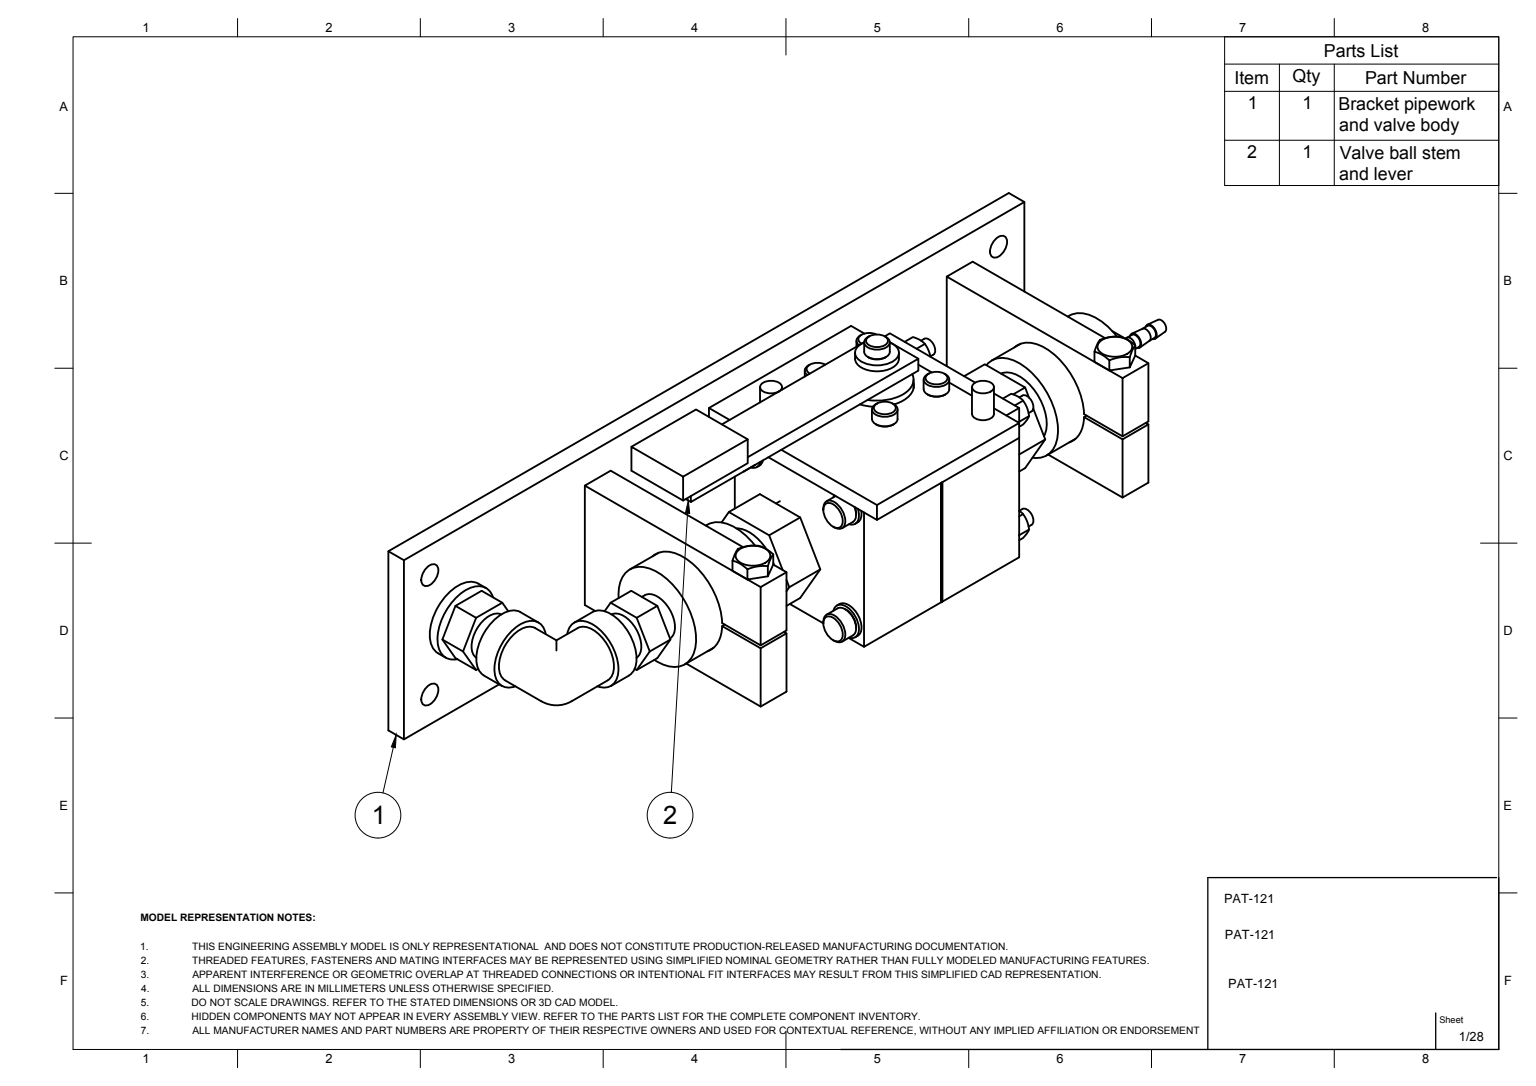
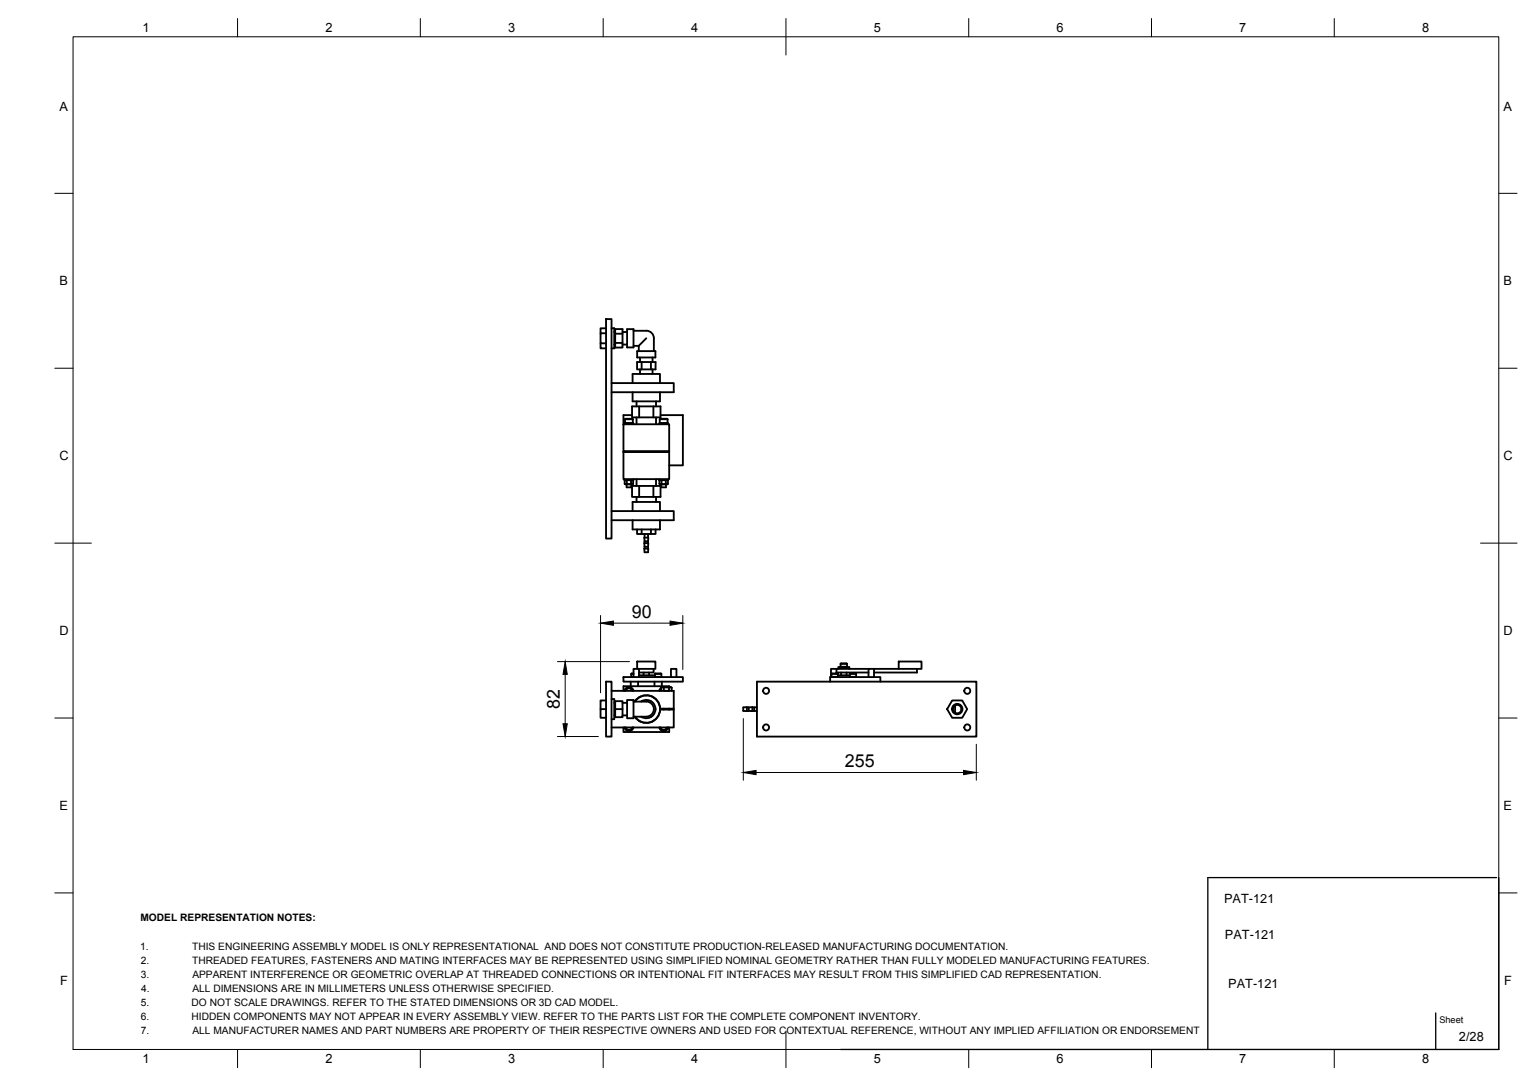
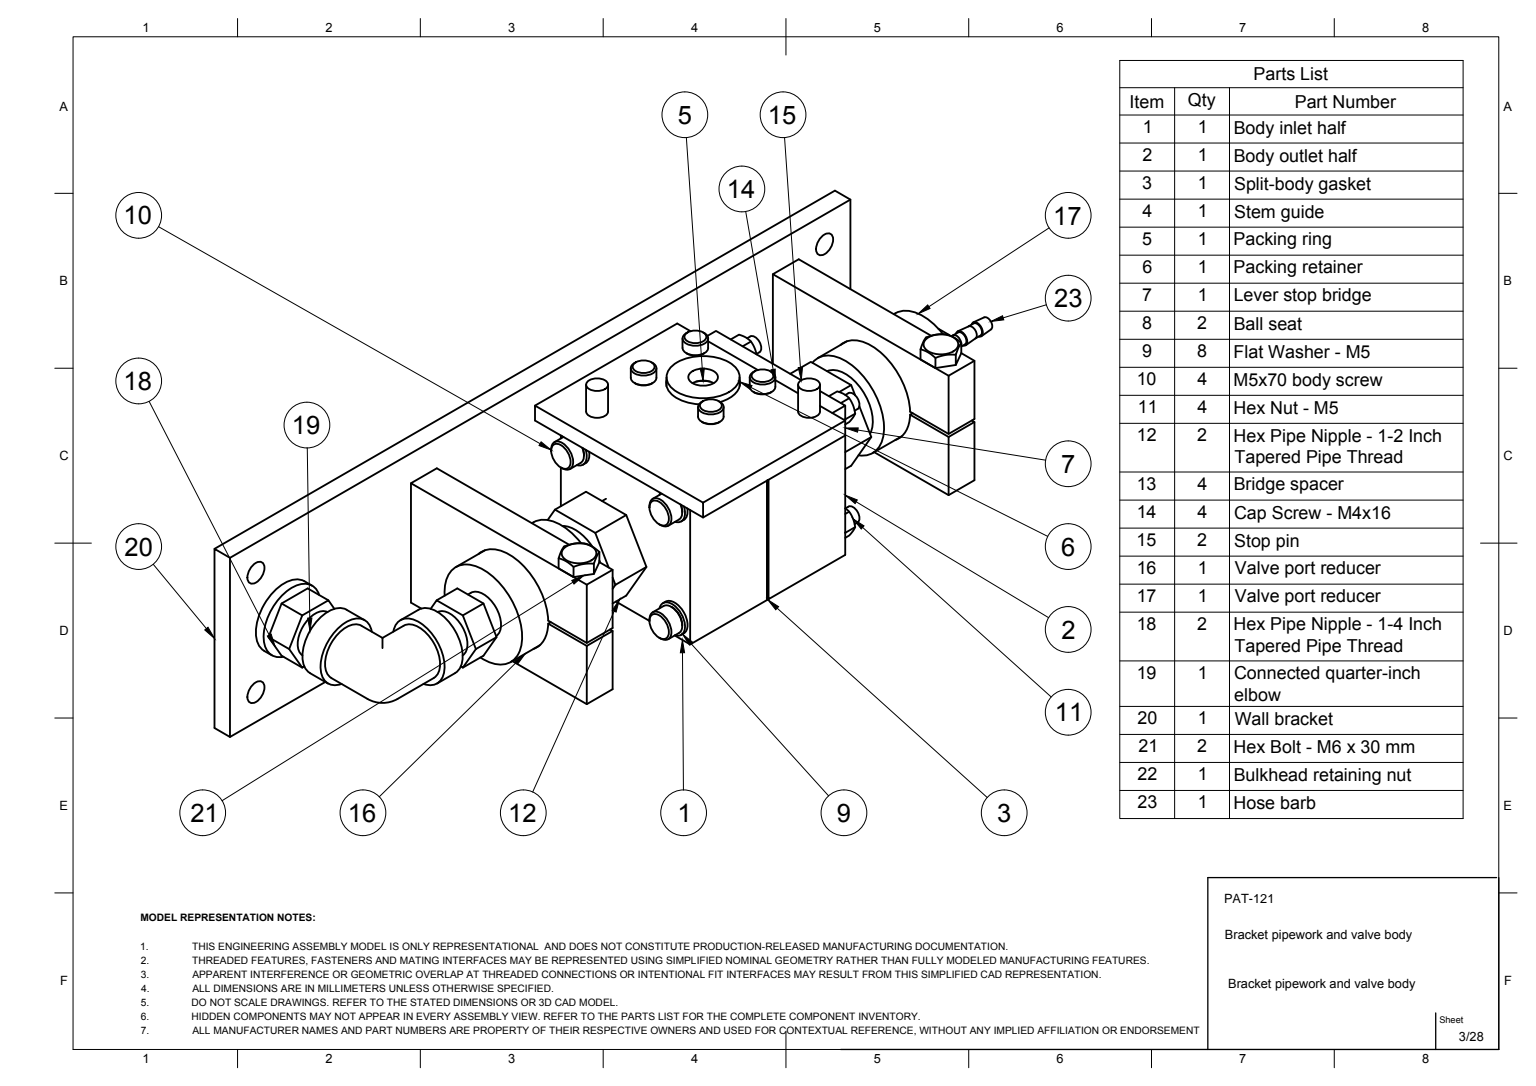
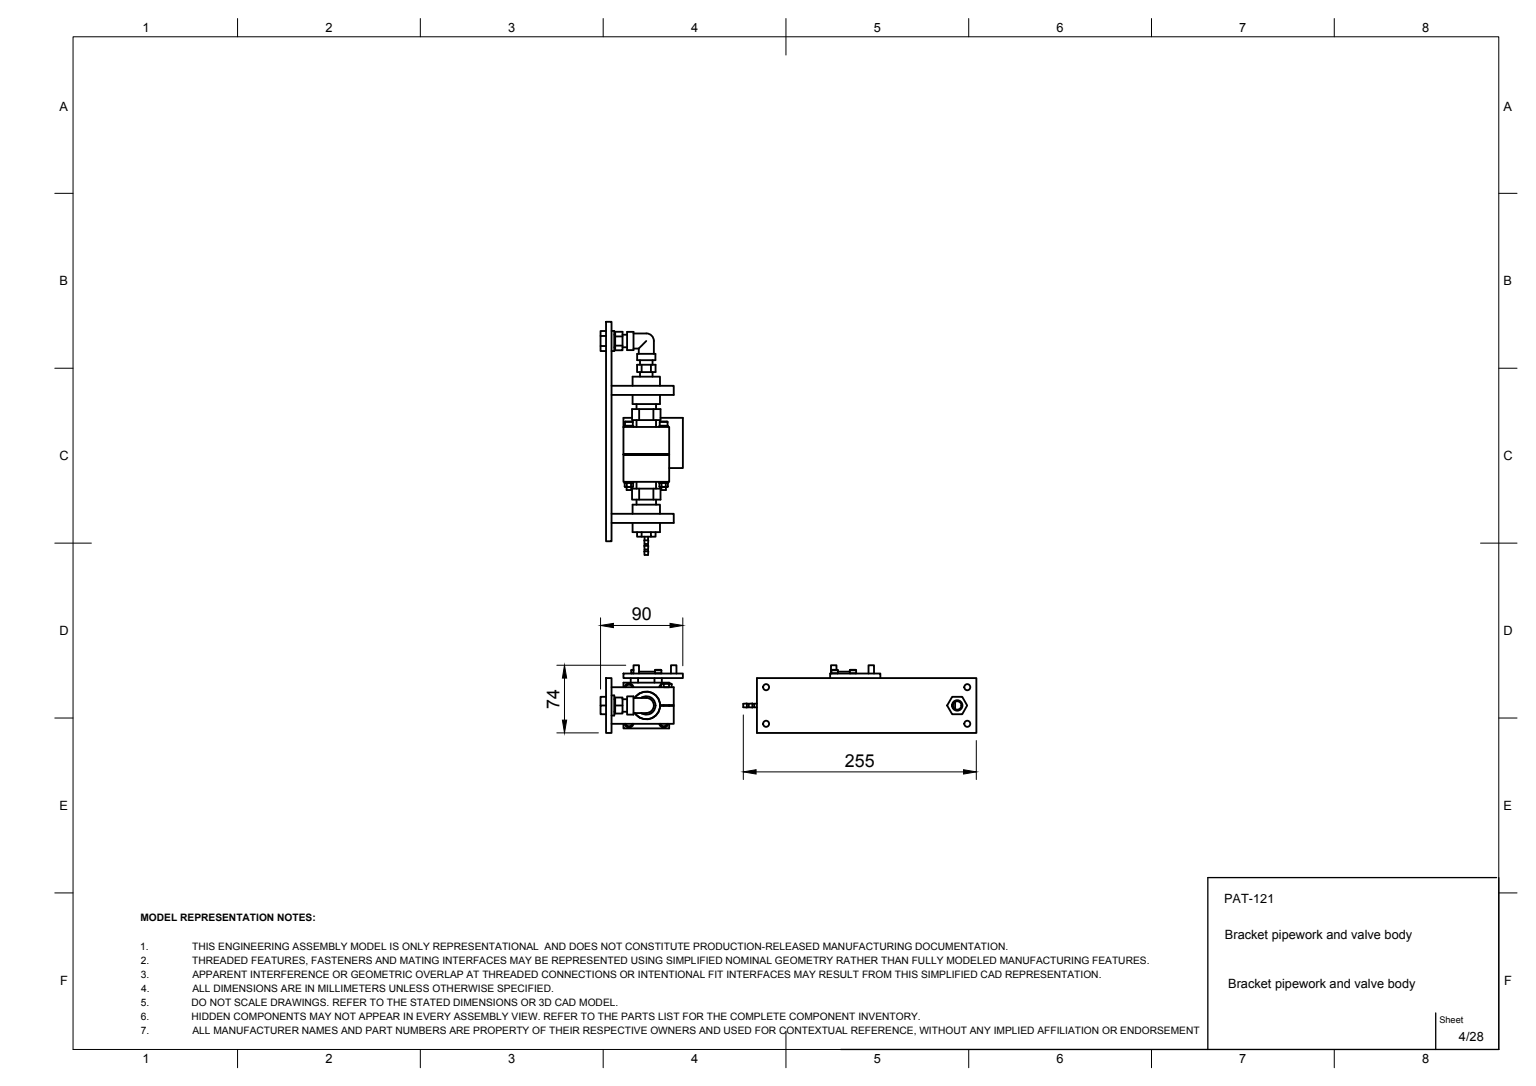
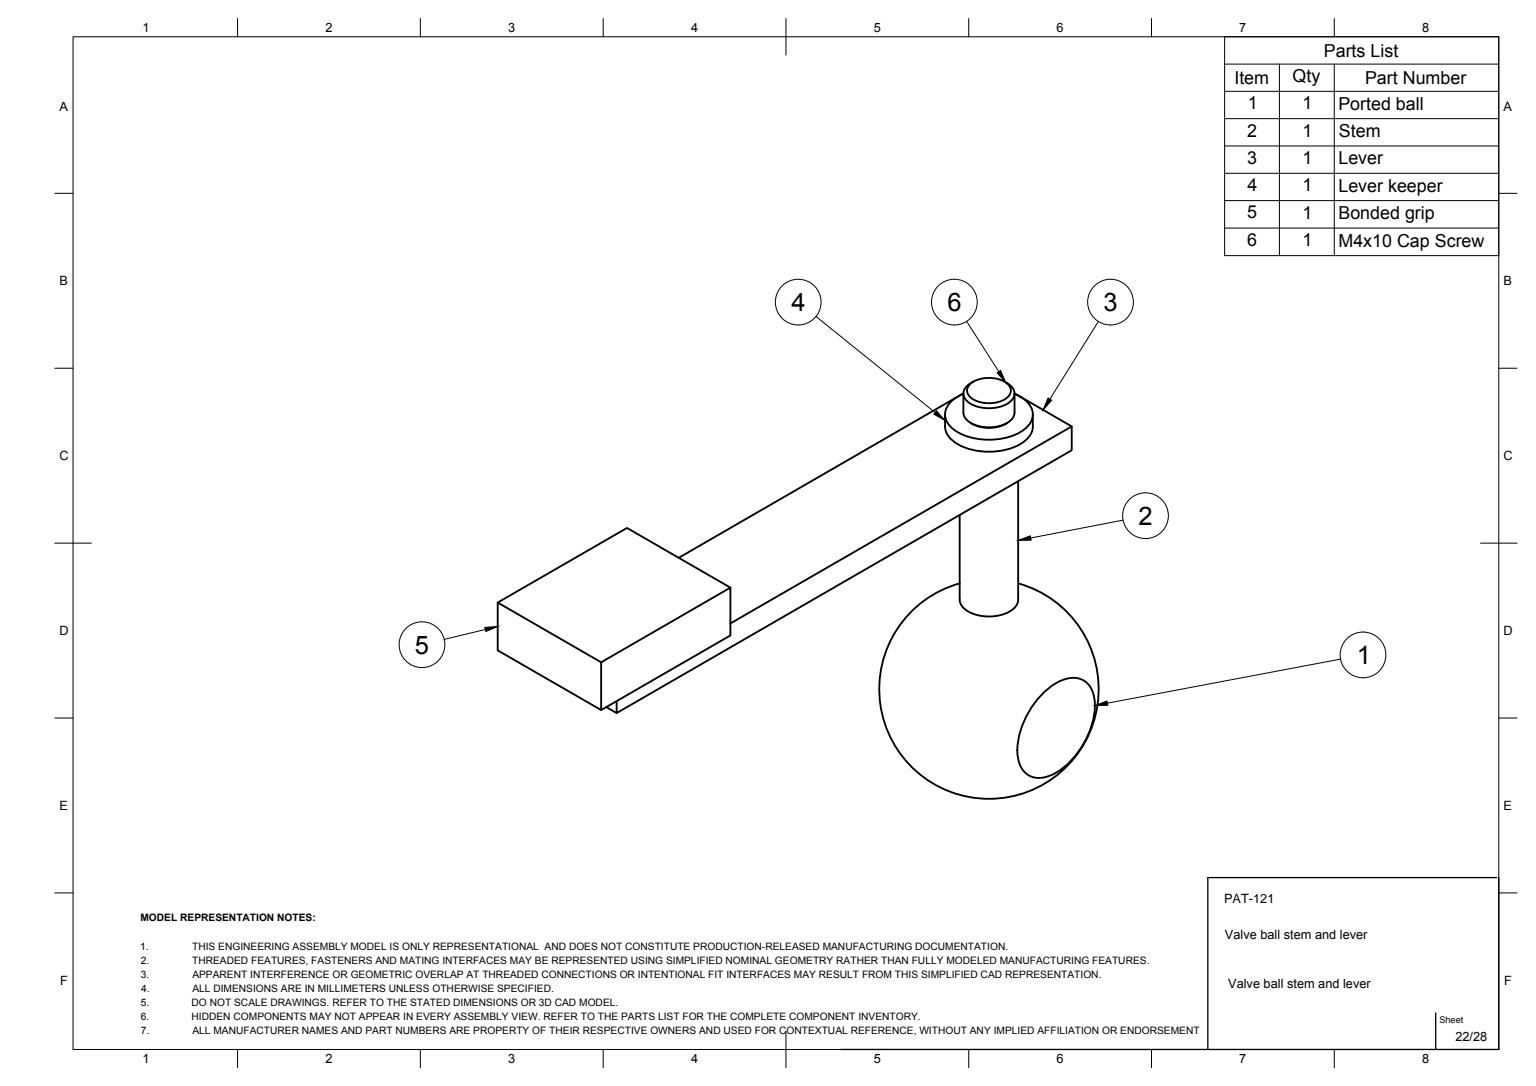
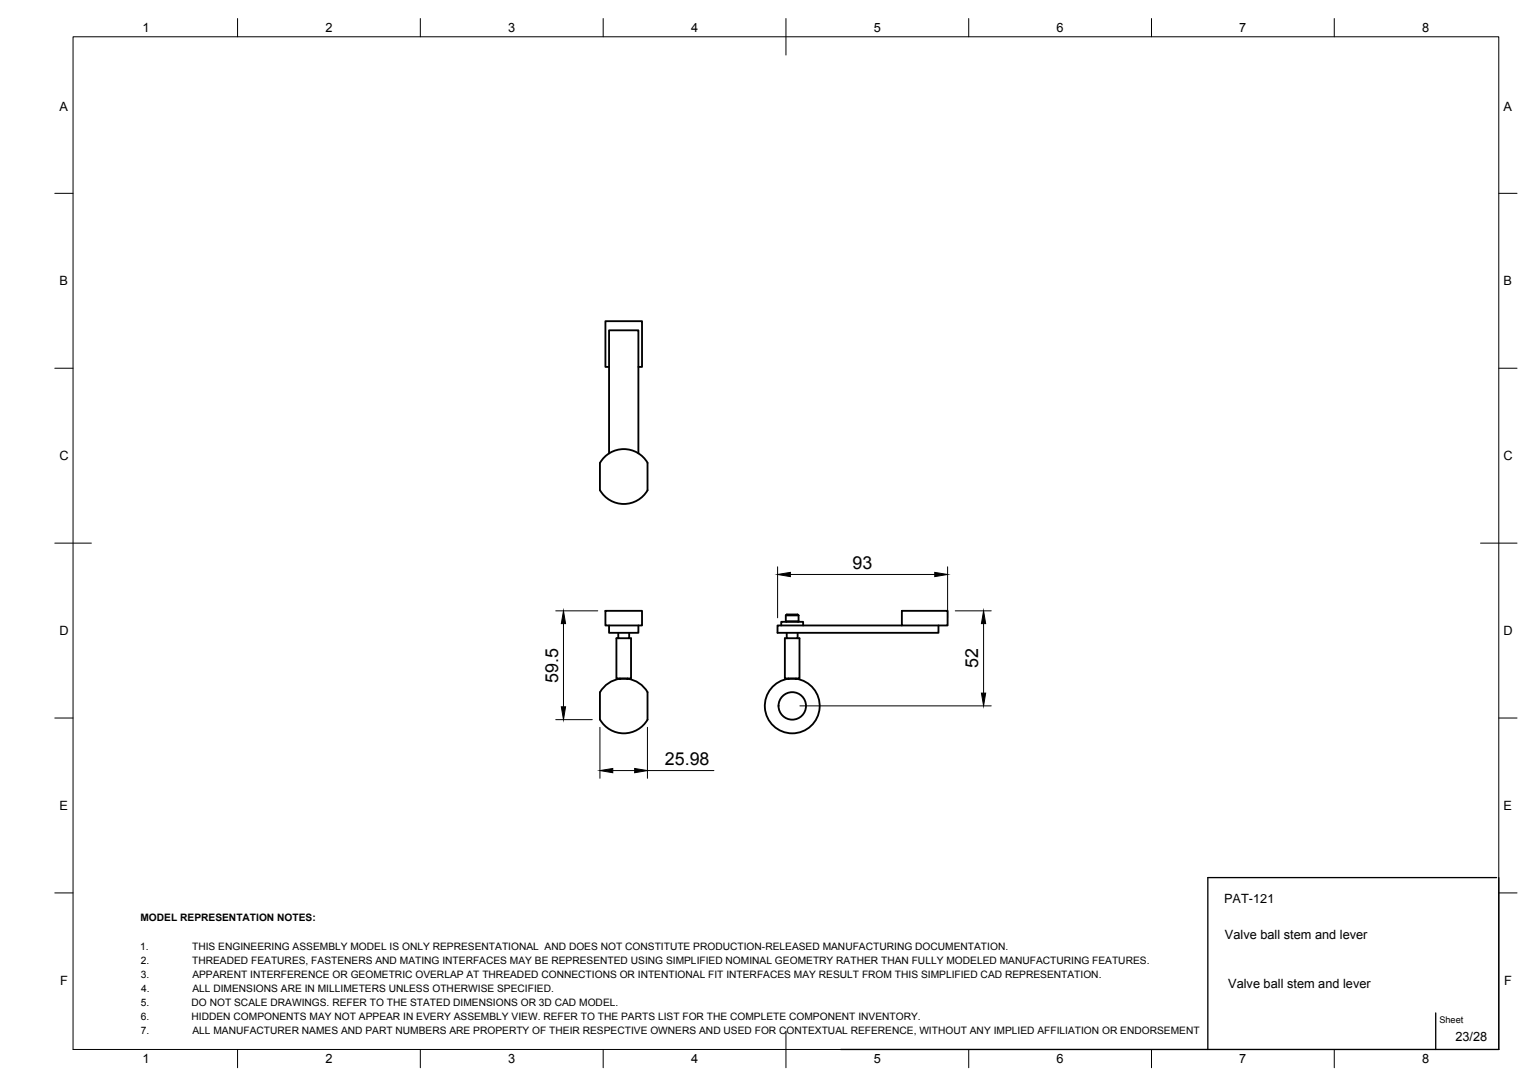
ISO-10303-21;
HEADER;
/* Generated by software containing ST-Developer
 * from STEP Tools, Inc. (www.steptools.com) 
 */

FILE_DESCRIPTION(
/* description */ ('Wall-mounted air drop station'),
/* implementation_level */ '2;1');

FILE_NAME(
/* name */ 'PAT-121',
/* time_stamp */ '2026-10-28T22:16:19-07:00',
/* author */ (''),
/* organization */ (''),
/* preprocessor_version */ 'ST-DEVELOPER v20.2',
/* originating_system */ 'Autodesk Translation Framework v15.17.0.0',
/* authorisation */ '');

FILE_SCHEMA (('AUTOMOTIVE_DESIGN { 1 0 10303 214 3 1 1 }'));
ENDSEC;

DATA;
#10=MECHANICAL_DESIGN_GEOMETRIC_PRESENTATION_REPRESENTATION('',(#344,#345,
#346,#347,#348,#349,#350,#351,#352,#353,#354,#355,#356,#357,#358,#359,#360,
#361,#362,#363,#364,#365,#366,#367,#368,#369,#370,#371,#372),#10517);
#11=ITEM_DEFINED_TRANSFORMATION($,$,#6237,#6766);
#12=ITEM_DEFINED_TRANSFORMATION($,$,#6254,#6767);
#13=ITEM_DEFINED_TRANSFORMATION($,$,#6271,#6768);
#14=ITEM_DEFINED_TRANSFORMATION($,$,#6333,#6769);
#15=ITEM_DEFINED_TRANSFORMATION($,$,#6345,#6770);
#16=ITEM_DEFINED_TRANSFORMATION($,$,#6381,#6771);
#17=ITEM_DEFINED_TRANSFORMATION($,$,#6424,#6772);
#18=ITEM_DEFINED_TRANSFORMATION($,$,#6467,#6773);
#19=ITEM_DEFINED_TRANSFORMATION($,$,#6494,#6774);
#20=ITEM_DEFINED_TRANSFORMATION($,$,#6507,#6775);
#21=ITEM_DEFINED_TRANSFORMATION($,$,#6511,#6776);
#22=ITEM_DEFINED_TRANSFORMATION($,$,#6524,#6777);
#23=ITEM_DEFINED_TRANSFORMATION($,$,#6554,#6778);
#24=ITEM_DEFINED_TRANSFORMATION($,$,#6554,#6779);
#25=ITEM_DEFINED_TRANSFORMATION($,$,#6593,#6780);
#26=ITEM_DEFINED_TRANSFORMATION($,$,#6565,#6781);
#27=ITEM_DEFINED_TRANSFORMATION($,$,#6593,#6782);
#28=ITEM_DEFINED_TRANSFORMATION($,$,#6604,#6783);
#29=ITEM_DEFINED_TRANSFORMATION($,$,#6593,#6784);
#30=ITEM_DEFINED_TRANSFORMATION($,$,#6565,#6785);
#31=ITEM_DEFINED_TRANSFORMATION($,$,#6593,#6786);
#32=ITEM_DEFINED_TRANSFORMATION($,$,#6604,#6787);
#33=ITEM_DEFINED_TRANSFORMATION($,$,#6593,#6788);
#34=ITEM_DEFINED_TRANSFORMATION($,$,#6565,#6789);
#35=ITEM_DEFINED_TRANSFORMATION($,$,#6593,#6790);
#36=ITEM_DEFINED_TRANSFORMATION($,$,#6604,#6791);
#37=ITEM_DEFINED_TRANSFORMATION($,$,#6593,#6792);
#38=ITEM_DEFINED_TRANSFORMATION($,$,#6565,#6793);
#39=ITEM_DEFINED_TRANSFORMATION($,$,#6593,#6794);
#40=ITEM_DEFINED_TRANSFORMATION($,$,#6604,#6795);
#41=ITEM_DEFINED_TRANSFORMATION($,$,#6620,#6796);
#42=ITEM_DEFINED_TRANSFORMATION($,$,#6620,#6797);
#43=ITEM_DEFINED_TRANSFORMATION($,$,#6644,#6798);
#44=ITEM_DEFINED_TRANSFORMATION($,$,#6653,#6799);
#45=ITEM_DEFINED_TRANSFORMATION($,$,#6644,#6800);
#46=ITEM_DEFINED_TRANSFORMATION($,$,#6653,#6801);
#47=ITEM_DEFINED_TRANSFORMATION($,$,#6644,#6802);
#48=ITEM_DEFINED_TRANSFORMATION($,$,#6653,#6803);
#49=ITEM_DEFINED_TRANSFORMATION($,$,#6644,#6804);
#50=ITEM_DEFINED_TRANSFORMATION($,$,#6653,#6805);
#51=ITEM_DEFINED_TRANSFORMATION($,$,#6679,#6806);
#52=ITEM_DEFINED_TRANSFORMATION($,$,#6679,#6807);
#53=ITEM_DEFINED_TRANSFORMATION($,$,#6725,#6808);
#54=ITEM_DEFINED_TRANSFORMATION($,$,#6685,#6809);
#55=ITEM_DEFINED_TRANSFORMATION($,$,#6725,#6810);
#56=ITEM_DEFINED_TRANSFORMATION($,$,#6749,#6811);
#57=ITEM_DEFINED_TRANSFORMATION($,$,#6749,#6812);
#58=ITEM_DEFINED_TRANSFORMATION($,$,#6814,#6916);
#59=ITEM_DEFINED_TRANSFORMATION($,$,#6830,#6917);
#60=ITEM_DEFINED_TRANSFORMATION($,$,#6865,#6918);
#61=ITEM_DEFINED_TRANSFORMATION($,$,#6876,#6919);
#62=ITEM_DEFINED_TRANSFORMATION($,$,#6885,#6920);
#63=ITEM_DEFINED_TRANSFORMATION($,$,#6892,#6921);
#64=ITEM_DEFINED_TRANSFORMATION($,$,#6236,#6922);
#65=ITEM_DEFINED_TRANSFORMATION($,$,#6813,#6923);
#66=(
REPRESENTATION_RELATIONSHIP($,$,#10643,#10642)
REPRESENTATION_RELATIONSHIP_WITH_TRANSFORMATION(#11)
SHAPE_REPRESENTATION_RELATIONSHIP()
);
#67=(
REPRESENTATION_RELATIONSHIP($,$,#10644,#10642)
REPRESENTATION_RELATIONSHIP_WITH_TRANSFORMATION(#12)
SHAPE_REPRESENTATION_RELATIONSHIP()
);
#68=(
REPRESENTATION_RELATIONSHIP($,$,#10645,#10642)
REPRESENTATION_RELATIONSHIP_WITH_TRANSFORMATION(#13)
SHAPE_REPRESENTATION_RELATIONSHIP()
);
#69=(
REPRESENTATION_RELATIONSHIP($,$,#10646,#10642)
REPRESENTATION_RELATIONSHIP_WITH_TRANSFORMATION(#14)
SHAPE_REPRESENTATION_RELATIONSHIP()
);
#70=(
REPRESENTATION_RELATIONSHIP($,$,#10647,#10642)
REPRESENTATION_RELATIONSHIP_WITH_TRANSFORMATION(#15)
SHAPE_REPRESENTATION_RELATIONSHIP()
);
#71=(
REPRESENTATION_RELATIONSHIP($,$,#10648,#10642)
REPRESENTATION_RELATIONSHIP_WITH_TRANSFORMATION(#16)
SHAPE_REPRESENTATION_RELATIONSHIP()
);
#72=(
REPRESENTATION_RELATIONSHIP($,$,#10649,#10642)
REPRESENTATION_RELATIONSHIP_WITH_TRANSFORMATION(#17)
SHAPE_REPRESENTATION_RELATIONSHIP()
);
#73=(
REPRESENTATION_RELATIONSHIP($,$,#10650,#10642)
REPRESENTATION_RELATIONSHIP_WITH_TRANSFORMATION(#18)
SHAPE_REPRESENTATION_RELATIONSHIP()
);
#74=(
REPRESENTATION_RELATIONSHIP($,$,#10651,#10642)
REPRESENTATION_RELATIONSHIP_WITH_TRANSFORMATION(#19)
SHAPE_REPRESENTATION_RELATIONSHIP()
);
#75=(
REPRESENTATION_RELATIONSHIP($,$,#10652,#10642)
REPRESENTATION_RELATIONSHIP_WITH_TRANSFORMATION(#20)
SHAPE_REPRESENTATION_RELATIONSHIP()
);
#76=(
REPRESENTATION_RELATIONSHIP($,$,#10653,#10642)
REPRESENTATION_RELATIONSHIP_WITH_TRANSFORMATION(#21)
SHAPE_REPRESENTATION_RELATIONSHIP()
);
#77=(
REPRESENTATION_RELATIONSHIP($,$,#10654,#10642)
REPRESENTATION_RELATIONSHIP_WITH_TRANSFORMATION(#22)
SHAPE_REPRESENTATION_RELATIONSHIP()
);
#78=(
REPRESENTATION_RELATIONSHIP($,$,#10655,#10642)
REPRESENTATION_RELATIONSHIP_WITH_TRANSFORMATION(#23)
SHAPE_REPRESENTATION_RELATIONSHIP()
);
#79=(
REPRESENTATION_RELATIONSHIP($,$,#10655,#10642)
REPRESENTATION_RELATIONSHIP_WITH_TRANSFORMATION(#24)
SHAPE_REPRESENTATION_RELATIONSHIP()
);
#80=(
REPRESENTATION_RELATIONSHIP($,$,#10657,#10642)
REPRESENTATION_RELATIONSHIP_WITH_TRANSFORMATION(#25)
SHAPE_REPRESENTATION_RELATIONSHIP()
);
#81=(
REPRESENTATION_RELATIONSHIP($,$,#10656,#10642)
REPRESENTATION_RELATIONSHIP_WITH_TRANSFORMATION(#26)
SHAPE_REPRESENTATION_RELATIONSHIP()
);
#82=(
REPRESENTATION_RELATIONSHIP($,$,#10657,#10642)
REPRESENTATION_RELATIONSHIP_WITH_TRANSFORMATION(#27)
SHAPE_REPRESENTATION_RELATIONSHIP()
);
#83=(
REPRESENTATION_RELATIONSHIP($,$,#10658,#10642)
REPRESENTATION_RELATIONSHIP_WITH_TRANSFORMATION(#28)
SHAPE_REPRESENTATION_RELATIONSHIP()
);
#84=(
REPRESENTATION_RELATIONSHIP($,$,#10657,#10642)
REPRESENTATION_RELATIONSHIP_WITH_TRANSFORMATION(#29)
SHAPE_REPRESENTATION_RELATIONSHIP()
);
#85=(
REPRESENTATION_RELATIONSHIP($,$,#10656,#10642)
REPRESENTATION_RELATIONSHIP_WITH_TRANSFORMATION(#30)
SHAPE_REPRESENTATION_RELATIONSHIP()
);
#86=(
REPRESENTATION_RELATIONSHIP($,$,#10657,#10642)
REPRESENTATION_RELATIONSHIP_WITH_TRANSFORMATION(#31)
SHAPE_REPRESENTATION_RELATIONSHIP()
);
#87=(
REPRESENTATION_RELATIONSHIP($,$,#10658,#10642)
REPRESENTATION_RELATIONSHIP_WITH_TRANSFORMATION(#32)
SHAPE_REPRESENTATION_RELATIONSHIP()
);
#88=(
REPRESENTATION_RELATIONSHIP($,$,#10657,#10642)
REPRESENTATION_RELATIONSHIP_WITH_TRANSFORMATION(#33)
SHAPE_REPRESENTATION_RELATIONSHIP()
);
#89=(
REPRESENTATION_RELATIONSHIP($,$,#10656,#10642)
REPRESENTATION_RELATIONSHIP_WITH_TRANSFORMATION(#34)
SHAPE_REPRESENTATION_RELATIONSHIP()
);
#90=(
REPRESENTATION_RELATIONSHIP($,$,#10657,#10642)
REPRESENTATION_RELATIONSHIP_WITH_TRANSFORMATION(#35)
SHAPE_REPRESENTATION_RELATIONSHIP()
);
#91=(
REPRESENTATION_RELATIONSHIP($,$,#10658,#10642)
REPRESENTATION_RELATIONSHIP_WITH_TRANSFORMATION(#36)
SHAPE_REPRESENTATION_RELATIONSHIP()
);
#92=(
REPRESENTATION_RELATIONSHIP($,$,#10657,#10642)
REPRESENTATION_RELATIONSHIP_WITH_TRANSFORMATION(#37)
SHAPE_REPRESENTATION_RELATIONSHIP()
);
#93=(
REPRESENTATION_RELATIONSHIP($,$,#10656,#10642)
REPRESENTATION_RELATIONSHIP_WITH_TRANSFORMATION(#38)
SHAPE_REPRESENTATION_RELATIONSHIP()
);
#94=(
REPRESENTATION_RELATIONSHIP($,$,#10657,#10642)
REPRESENTATION_RELATIONSHIP_WITH_TRANSFORMATION(#39)
SHAPE_REPRESENTATION_RELATIONSHIP()
);
#95=(
REPRESENTATION_RELATIONSHIP($,$,#10658,#10642)
REPRESENTATION_RELATIONSHIP_WITH_TRANSFORMATION(#40)
SHAPE_REPRESENTATION_RELATIONSHIP()
);
#96=(
REPRESENTATION_RELATIONSHIP($,$,#10659,#10642)
REPRESENTATION_RELATIONSHIP_WITH_TRANSFORMATION(#41)
SHAPE_REPRESENTATION_RELATIONSHIP()
);
#97=(
REPRESENTATION_RELATIONSHIP($,$,#10659,#10642)
REPRESENTATION_RELATIONSHIP_WITH_TRANSFORMATION(#42)
SHAPE_REPRESENTATION_RELATIONSHIP()
);
#98=(
REPRESENTATION_RELATIONSHIP($,$,#10660,#10642)
REPRESENTATION_RELATIONSHIP_WITH_TRANSFORMATION(#43)
SHAPE_REPRESENTATION_RELATIONSHIP()
);
#99=(
REPRESENTATION_RELATIONSHIP($,$,#10661,#10642)
REPRESENTATION_RELATIONSHIP_WITH_TRANSFORMATION(#44)
SHAPE_REPRESENTATION_RELATIONSHIP()
);
#100=(
REPRESENTATION_RELATIONSHIP($,$,#10660,#10642)
REPRESENTATION_RELATIONSHIP_WITH_TRANSFORMATION(#45)
SHAPE_REPRESENTATION_RELATIONSHIP()
);
#101=(
REPRESENTATION_RELATIONSHIP($,$,#10661,#10642)
REPRESENTATION_RELATIONSHIP_WITH_TRANSFORMATION(#46)
SHAPE_REPRESENTATION_RELATIONSHIP()
);
#102=(
REPRESENTATION_RELATIONSHIP($,$,#10660,#10642)
REPRESENTATION_RELATIONSHIP_WITH_TRANSFORMATION(#47)
SHAPE_REPRESENTATION_RELATIONSHIP()
);
#103=(
REPRESENTATION_RELATIONSHIP($,$,#10661,#10642)
REPRESENTATION_RELATIONSHIP_WITH_TRANSFORMATION(#48)
SHAPE_REPRESENTATION_RELATIONSHIP()
);
#104=(
REPRESENTATION_RELATIONSHIP($,$,#10660,#10642)
REPRESENTATION_RELATIONSHIP_WITH_TRANSFORMATION(#49)
SHAPE_REPRESENTATION_RELATIONSHIP()
);
#105=(
REPRESENTATION_RELATIONSHIP($,$,#10661,#10642)
REPRESENTATION_RELATIONSHIP_WITH_TRANSFORMATION(#50)
SHAPE_REPRESENTATION_RELATIONSHIP()
);
#106=(
REPRESENTATION_RELATIONSHIP($,$,#10662,#10642)
REPRESENTATION_RELATIONSHIP_WITH_TRANSFORMATION(#51)
SHAPE_REPRESENTATION_RELATIONSHIP()
);
#107=(
REPRESENTATION_RELATIONSHIP($,$,#10662,#10642)
REPRESENTATION_RELATIONSHIP_WITH_TRANSFORMATION(#52)
SHAPE_REPRESENTATION_RELATIONSHIP()
);
#108=(
REPRESENTATION_RELATIONSHIP($,$,#10664,#10642)
REPRESENTATION_RELATIONSHIP_WITH_TRANSFORMATION(#53)
SHAPE_REPRESENTATION_RELATIONSHIP()
);
#109=(
REPRESENTATION_RELATIONSHIP($,$,#10663,#10642)
REPRESENTATION_RELATIONSHIP_WITH_TRANSFORMATION(#54)
SHAPE_REPRESENTATION_RELATIONSHIP()
);
#110=(
REPRESENTATION_RELATIONSHIP($,$,#10664,#10642)
REPRESENTATION_RELATIONSHIP_WITH_TRANSFORMATION(#55)
SHAPE_REPRESENTATION_RELATIONSHIP()
);
#111=(
REPRESENTATION_RELATIONSHIP($,$,#10665,#10642)
REPRESENTATION_RELATIONSHIP_WITH_TRANSFORMATION(#56)
SHAPE_REPRESENTATION_RELATIONSHIP()
);
#112=(
REPRESENTATION_RELATIONSHIP($,$,#10665,#10642)
REPRESENTATION_RELATIONSHIP_WITH_TRANSFORMATION(#57)
SHAPE_REPRESENTATION_RELATIONSHIP()
);
#113=(
REPRESENTATION_RELATIONSHIP($,$,#10667,#10666)
REPRESENTATION_RELATIONSHIP_WITH_TRANSFORMATION(#58)
SHAPE_REPRESENTATION_RELATIONSHIP()
);
#114=(
REPRESENTATION_RELATIONSHIP($,$,#10668,#10666)
REPRESENTATION_RELATIONSHIP_WITH_TRANSFORMATION(#59)
SHAPE_REPRESENTATION_RELATIONSHIP()
);
#115=(
REPRESENTATION_RELATIONSHIP($,$,#10669,#10666)
REPRESENTATION_RELATIONSHIP_WITH_TRANSFORMATION(#60)
SHAPE_REPRESENTATION_RELATIONSHIP()
);
#116=(
REPRESENTATION_RELATIONSHIP($,$,#10670,#10666)
REPRESENTATION_RELATIONSHIP_WITH_TRANSFORMATION(#61)
SHAPE_REPRESENTATION_RELATIONSHIP()
);
#117=(
REPRESENTATION_RELATIONSHIP($,$,#10671,#10666)
REPRESENTATION_RELATIONSHIP_WITH_TRANSFORMATION(#62)
SHAPE_REPRESENTATION_RELATIONSHIP()
);
#118=(
REPRESENTATION_RELATIONSHIP($,$,#10672,#10666)
REPRESENTATION_RELATIONSHIP_WITH_TRANSFORMATION(#63)
SHAPE_REPRESENTATION_RELATIONSHIP()
);
#119=(
REPRESENTATION_RELATIONSHIP($,$,#10642,#10641)
REPRESENTATION_RELATIONSHIP_WITH_TRANSFORMATION(#64)
SHAPE_REPRESENTATION_RELATIONSHIP()
);
#120=(
REPRESENTATION_RELATIONSHIP($,$,#10666,#10641)
REPRESENTATION_RELATIONSHIP_WITH_TRANSFORMATION(#65)
SHAPE_REPRESENTATION_RELATIONSHIP()
);
#121=CONTEXT_DEPENDENT_SHAPE_REPRESENTATION(#66,#10579);
#122=CONTEXT_DEPENDENT_SHAPE_REPRESENTATION(#67,#10580);
#123=CONTEXT_DEPENDENT_SHAPE_REPRESENTATION(#68,#10581);
#124=CONTEXT_DEPENDENT_SHAPE_REPRESENTATION(#69,#10582);
#125=CONTEXT_DEPENDENT_SHAPE_REPRESENTATION(#70,#10583);
#126=CONTEXT_DEPENDENT_SHAPE_REPRESENTATION(#71,#10584);
#127=CONTEXT_DEPENDENT_SHAPE_REPRESENTATION(#72,#10585);
#128=CONTEXT_DEPENDENT_SHAPE_REPRESENTATION(#73,#10586);
#129=CONTEXT_DEPENDENT_SHAPE_REPRESENTATION(#74,#10587);
#130=CONTEXT_DEPENDENT_SHAPE_REPRESENTATION(#75,#10588);
#131=CONTEXT_DEPENDENT_SHAPE_REPRESENTATION(#76,#10589);
#132=CONTEXT_DEPENDENT_SHAPE_REPRESENTATION(#77,#10590);
#133=CONTEXT_DEPENDENT_SHAPE_REPRESENTATION(#78,#10591);
#134=CONTEXT_DEPENDENT_SHAPE_REPRESENTATION(#79,#10592);
#135=CONTEXT_DEPENDENT_SHAPE_REPRESENTATION(#80,#10593);
#136=CONTEXT_DEPENDENT_SHAPE_REPRESENTATION(#81,#10594);
#137=CONTEXT_DEPENDENT_SHAPE_REPRESENTATION(#82,#10595);
#138=CONTEXT_DEPENDENT_SHAPE_REPRESENTATION(#83,#10596);
#139=CONTEXT_DEPENDENT_SHAPE_REPRESENTATION(#84,#10597);
#140=CONTEXT_DEPENDENT_SHAPE_REPRESENTATION(#85,#10598);
#141=CONTEXT_DEPENDENT_SHAPE_REPRESENTATION(#86,#10599);
#142=CONTEXT_DEPENDENT_SHAPE_REPRESENTATION(#87,#10600);
#143=CONTEXT_DEPENDENT_SHAPE_REPRESENTATION(#88,#10601);
#144=CONTEXT_DEPENDENT_SHAPE_REPRESENTATION(#89,#10602);
#145=CONTEXT_DEPENDENT_SHAPE_REPRESENTATION(#90,#10603);
#146=CONTEXT_DEPENDENT_SHAPE_REPRESENTATION(#91,#10604);
#147=CONTEXT_DEPENDENT_SHAPE_REPRESENTATION(#92,#10605);
#148=CONTEXT_DEPENDENT_SHAPE_REPRESENTATION(#93,#10606);
#149=CONTEXT_DEPENDENT_SHAPE_REPRESENTATION(#94,#10607);
#150=CONTEXT_DEPENDENT_SHAPE_REPRESENTATION(#95,#10608);
#151=CONTEXT_DEPENDENT_SHAPE_REPRESENTATION(#96,#10609);
#152=CONTEXT_DEPENDENT_SHAPE_REPRESENTATION(#97,#10610);
#153=CONTEXT_DEPENDENT_SHAPE_REPRESENTATION(#98,#10611);
#154=CONTEXT_DEPENDENT_SHAPE_REPRESENTATION(#99,#10612);
#155=CONTEXT_DEPENDENT_SHAPE_REPRESENTATION(#100,#10613);
#156=CONTEXT_DEPENDENT_SHAPE_REPRESENTATION(#101,#10614);
#157=CONTEXT_DEPENDENT_SHAPE_REPRESENTATION(#102,#10615);
#158=CONTEXT_DEPENDENT_SHAPE_REPRESENTATION(#103,#10616);
#159=CONTEXT_DEPENDENT_SHAPE_REPRESENTATION(#104,#10617);
#160=CONTEXT_DEPENDENT_SHAPE_REPRESENTATION(#105,#10618);
#161=CONTEXT_DEPENDENT_SHAPE_REPRESENTATION(#106,#10619);
#162=CONTEXT_DEPENDENT_SHAPE_REPRESENTATION(#107,#10620);
#163=CONTEXT_DEPENDENT_SHAPE_REPRESENTATION(#108,#10621);
#164=CONTEXT_DEPENDENT_SHAPE_REPRESENTATION(#109,#10622);
#165=CONTEXT_DEPENDENT_SHAPE_REPRESENTATION(#110,#10623);
#166=CONTEXT_DEPENDENT_SHAPE_REPRESENTATION(#111,#10624);
#167=CONTEXT_DEPENDENT_SHAPE_REPRESENTATION(#112,#10625);
#168=CONTEXT_DEPENDENT_SHAPE_REPRESENTATION(#113,#10633);
#169=CONTEXT_DEPENDENT_SHAPE_REPRESENTATION(#114,#10634);
#170=CONTEXT_DEPENDENT_SHAPE_REPRESENTATION(#115,#10635);
#171=CONTEXT_DEPENDENT_SHAPE_REPRESENTATION(#116,#10636);
#172=CONTEXT_DEPENDENT_SHAPE_REPRESENTATION(#117,#10637);
#173=CONTEXT_DEPENDENT_SHAPE_REPRESENTATION(#118,#10638);
#174=CONTEXT_DEPENDENT_SHAPE_REPRESENTATION(#119,#10639);
#175=CONTEXT_DEPENDENT_SHAPE_REPRESENTATION(#120,#10640);
#176=NEXT_ASSEMBLY_USAGE_OCCURRENCE('Valve port reducer:1',
'Valve port reducer:1','Valve port reducer:1',#10675,#10676,
'Valve port reducer:1');
#177=NEXT_ASSEMBLY_USAGE_OCCURRENCE('Valve port reducer (1):1',
'Valve port reducer (1):1','Valve port reducer (1):1',#10675,#10677,
'Valve port reducer (1):1');
#178=NEXT_ASSEMBLY_USAGE_OCCURRENCE('Wall bracket:1','Wall bracket:1',
'Wall bracket:1',#10675,#10678,'Wall bracket:1');
#179=NEXT_ASSEMBLY_USAGE_OCCURRENCE('Bulkhead retaining nut:1',
'Bulkhead retaining nut:1','Bulkhead retaining nut:1',#10675,#10679,
'Bulkhead retaining nut:1');
#180=NEXT_ASSEMBLY_USAGE_OCCURRENCE('Hose barb:1','Hose barb:1',
'Hose barb:1',#10675,#10680,'Hose barb:1');
#181=NEXT_ASSEMBLY_USAGE_OCCURRENCE('Body inlet half:2',
'Body inlet half:2','Body inlet half:2',#10675,#10681,
'Body inlet half:2');
#182=NEXT_ASSEMBLY_USAGE_OCCURRENCE('Body outlet half:2',
'Body outlet half:2','Body outlet half:2',#10675,#10682,
'Body outlet half:2');
#183=NEXT_ASSEMBLY_USAGE_OCCURRENCE('Split-body gasket:2',
'Split-body gasket:2','Split-body gasket:2',#10675,#10683,
'Split-body gasket:2');
#184=NEXT_ASSEMBLY_USAGE_OCCURRENCE('Stem guide:2','Stem guide:2',
'Stem guide:2',#10675,#10684,'Stem guide:2');
#185=NEXT_ASSEMBLY_USAGE_OCCURRENCE('Packing ring:2','Packing ring:2',
'Packing ring:2',#10675,#10685,'Packing ring:2');
#186=NEXT_ASSEMBLY_USAGE_OCCURRENCE('Packing retainer:2',
'Packing retainer:2','Packing retainer:2',#10675,#10686,
'Packing retainer:2');
#187=NEXT_ASSEMBLY_USAGE_OCCURRENCE('Lever stop bridge:2',
'Lever stop bridge:2','Lever stop bridge:2',#10675,#10687,
'Lever stop bridge:2');
#188=NEXT_ASSEMBLY_USAGE_OCCURRENCE('Ball seat:2','Ball seat:2',
'Ball seat:2',#10675,#10688,'Ball seat:2');
#189=NEXT_ASSEMBLY_USAGE_OCCURRENCE('Ball seat:3','Ball seat:3',
'Ball seat:3',#10675,#10688,'Ball seat:3');
#190=NEXT_ASSEMBLY_USAGE_OCCURRENCE('Flat Washer - M5:2',
'Flat Washer - M5:2','Flat Washer - M5:2',#10675,#10690,
'Flat Washer - M5:2');
#191=NEXT_ASSEMBLY_USAGE_OCCURRENCE('M5x70 body screw:2',
'M5x70 body screw:2','M5x70 body screw:2',#10675,#10689,
'M5x70 body screw:2');
#192=NEXT_ASSEMBLY_USAGE_OCCURRENCE('Flat Washer - M5:3',
'Flat Washer - M5:3','Flat Washer - M5:3',#10675,#10690,
'Flat Washer - M5:3');
#193=NEXT_ASSEMBLY_USAGE_OCCURRENCE('Hex Nut - M5:2','Hex Nut - M5:2',
'Hex Nut - M5:2',#10675,#10691,'Hex Nut - M5:2');
#194=NEXT_ASSEMBLY_USAGE_OCCURRENCE('Flat Washer - M5:4',
'Flat Washer - M5:4','Flat Washer - M5:4',#10675,#10690,
'Flat Washer - M5:4');
#195=NEXT_ASSEMBLY_USAGE_OCCURRENCE('M5x70 body screw:3',
'M5x70 body screw:3','M5x70 body screw:3',#10675,#10689,
'M5x70 body screw:3');
#196=NEXT_ASSEMBLY_USAGE_OCCURRENCE('Flat Washer - M5:5',
'Flat Washer - M5:5','Flat Washer - M5:5',#10675,#10690,
'Flat Washer - M5:5');
#197=NEXT_ASSEMBLY_USAGE_OCCURRENCE('Hex Nut - M5:3','Hex Nut - M5:3',
'Hex Nut - M5:3',#10675,#10691,'Hex Nut - M5:3');
#198=NEXT_ASSEMBLY_USAGE_OCCURRENCE('Flat Washer - M5:6',
'Flat Washer - M5:6','Flat Washer - M5:6',#10675,#10690,
'Flat Washer - M5:6');
#199=NEXT_ASSEMBLY_USAGE_OCCURRENCE('M5x70 body screw:4',
'M5x70 body screw:4','M5x70 body screw:4',#10675,#10689,
'M5x70 body screw:4');
#200=NEXT_ASSEMBLY_USAGE_OCCURRENCE('Flat Washer - M5:7',
'Flat Washer - M5:7','Flat Washer - M5:7',#10675,#10690,
'Flat Washer - M5:7');
#201=NEXT_ASSEMBLY_USAGE_OCCURRENCE('Hex Nut - M5:4','Hex Nut - M5:4',
'Hex Nut - M5:4',#10675,#10691,'Hex Nut - M5:4');
#202=NEXT_ASSEMBLY_USAGE_OCCURRENCE('Flat Washer - M5:8',
'Flat Washer - M5:8','Flat Washer - M5:8',#10675,#10690,
'Flat Washer - M5:8');
#203=NEXT_ASSEMBLY_USAGE_OCCURRENCE('M5x70 body screw:5',
'M5x70 body screw:5','M5x70 body screw:5',#10675,#10689,
'M5x70 body screw:5');
#204=NEXT_ASSEMBLY_USAGE_OCCURRENCE('Flat Washer - M5:9',
'Flat Washer - M5:9','Flat Washer - M5:9',#10675,#10690,
'Flat Washer - M5:9');
#205=NEXT_ASSEMBLY_USAGE_OCCURRENCE('Hex Nut - M5:5','Hex Nut - M5:5',
'Hex Nut - M5:5',#10675,#10691,'Hex Nut - M5:5');
#206=NEXT_ASSEMBLY_USAGE_OCCURRENCE(
'Hex Pipe Nipple - 1-2 Inch Tapered Pipe Thread:2',
'Hex Pipe Nipple - 1-2 Inch Tapered Pipe Thread:2',
'Hex Pipe Nipple - 1-2 Inch Tapered Pipe Thread:2',#10675,#10692,
'Hex Pipe Nipple - 1-2 Inch Tapered Pipe Thread:2');
#207=NEXT_ASSEMBLY_USAGE_OCCURRENCE(
'Hex Pipe Nipple - 1-2 Inch Tapered Pipe Thread:3',
'Hex Pipe Nipple - 1-2 Inch Tapered Pipe Thread:3',
'Hex Pipe Nipple - 1-2 Inch Tapered Pipe Thread:3',#10675,#10692,
'Hex Pipe Nipple - 1-2 Inch Tapered Pipe Thread:3');
#208=NEXT_ASSEMBLY_USAGE_OCCURRENCE('Bridge spacer:2','Bridge spacer:2',
'Bridge spacer:2',#10675,#10693,'Bridge spacer:2');
#209=NEXT_ASSEMBLY_USAGE_OCCURRENCE('Cap Screw - M4x16:2',
'Cap Screw - M4x16:2','Cap Screw - M4x16:2',#10675,#10694,
'Cap Screw - M4x16:2');
#210=NEXT_ASSEMBLY_USAGE_OCCURRENCE('Bridge spacer:3','Bridge spacer:3',
'Bridge spacer:3',#10675,#10693,'Bridge spacer:3');
#211=NEXT_ASSEMBLY_USAGE_OCCURRENCE('Cap Screw - M4x16:3',
'Cap Screw - M4x16:3','Cap Screw - M4x16:3',#10675,#10694,
'Cap Screw - M4x16:3');
#212=NEXT_ASSEMBLY_USAGE_OCCURRENCE('Bridge spacer:4','Bridge spacer:4',
'Bridge spacer:4',#10675,#10693,'Bridge spacer:4');
#213=NEXT_ASSEMBLY_USAGE_OCCURRENCE('Cap Screw - M4x16:4',
'Cap Screw - M4x16:4','Cap Screw - M4x16:4',#10675,#10694,
'Cap Screw - M4x16:4');
#214=NEXT_ASSEMBLY_USAGE_OCCURRENCE('Bridge spacer:5','Bridge spacer:5',
'Bridge spacer:5',#10675,#10693,'Bridge spacer:5');
#215=NEXT_ASSEMBLY_USAGE_OCCURRENCE('Cap Screw - M4x16:5',
'Cap Screw - M4x16:5','Cap Screw - M4x16:5',#10675,#10694,
'Cap Screw - M4x16:5');
#216=NEXT_ASSEMBLY_USAGE_OCCURRENCE('Stop pin:2','Stop pin:2',
'Stop pin:2',#10675,#10695,'Stop pin:2');
#217=NEXT_ASSEMBLY_USAGE_OCCURRENCE('Stop pin:3','Stop pin:3',
'Stop pin:3',#10675,#10695,'Stop pin:3');
#218=NEXT_ASSEMBLY_USAGE_OCCURRENCE(
'Hex Pipe Nipple - 1-4 Inch Tapered Pipe Thread:2',
'Hex Pipe Nipple - 1-4 Inch Tapered Pipe Thread:2',
'Hex Pipe Nipple - 1-4 Inch Tapered Pipe Thread:2',#10675,#10697,
'Hex Pipe Nipple - 1-4 Inch Tapered Pipe Thread:2');
#219=NEXT_ASSEMBLY_USAGE_OCCURRENCE('Connected quarter-inch elbow:2',
'Connected quarter-inch elbow:2','Connected quarter-inch elbow:2',#10675,
#10696,'Connected quarter-inch elbow:2');
#220=NEXT_ASSEMBLY_USAGE_OCCURRENCE(
'Hex Pipe Nipple - 1-4 Inch Tapered Pipe Thread:3',
'Hex Pipe Nipple - 1-4 Inch Tapered Pipe Thread:3',
'Hex Pipe Nipple - 1-4 Inch Tapered Pipe Thread:3',#10675,#10697,
'Hex Pipe Nipple - 1-4 Inch Tapered Pipe Thread:3');
#221=NEXT_ASSEMBLY_USAGE_OCCURRENCE('Hex Bolt - M6 x 30 mm:2',
'Hex Bolt - M6 x 30 mm:2','Hex Bolt - M6 x 30 mm:2',#10675,#10698,
'Hex Bolt - M6 x 30 mm:2');
#222=NEXT_ASSEMBLY_USAGE_OCCURRENCE('Hex Bolt - M6 x 30 mm:3',
'Hex Bolt - M6 x 30 mm:3','Hex Bolt - M6 x 30 mm:3',#10675,#10698,
'Hex Bolt - M6 x 30 mm:3');
#223=NEXT_ASSEMBLY_USAGE_OCCURRENCE('Ported ball:2','Ported ball:2',
'Ported ball:2',#10699,#10700,'Ported ball:2');
#224=NEXT_ASSEMBLY_USAGE_OCCURRENCE('Stem:2','Stem:2','Stem:2',#10699,#10701,
'Stem:2');
#225=NEXT_ASSEMBLY_USAGE_OCCURRENCE('Lever:2','Lever:2','Lever:2',#10699,
#10702,'Lever:2');
#226=NEXT_ASSEMBLY_USAGE_OCCURRENCE('Lever keeper:2','Lever keeper:2',
'Lever keeper:2',#10699,#10703,'Lever keeper:2');
#227=NEXT_ASSEMBLY_USAGE_OCCURRENCE('Bonded grip:2','Bonded grip:2',
'Bonded grip:2',#10699,#10704,'Bonded grip:2');
#228=NEXT_ASSEMBLY_USAGE_OCCURRENCE('M4x10 Cap Screw:2',
'M4x10 Cap Screw:2','M4x10 Cap Screw:2',#10699,#10705,
'M4x10 Cap Screw:2');
#229=NEXT_ASSEMBLY_USAGE_OCCURRENCE('Bracket pipework and valve body:1',
'Bracket pipework and valve body:1','Bracket pipework and valve body:1',
#10674,#10675,'Bracket pipework and valve body:1');
#230=NEXT_ASSEMBLY_USAGE_OCCURRENCE('Valve ball stem and lever:1',
'Valve ball stem and lever:1','Valve ball stem and lever:1',#10674,#10699,
'Valve ball stem and lever:1');
#231=ELLIPSE('',#6687,0.650538238691624,0.46);
#232=ELLIPSE('',#6711,1.1667261889578,0.825);
#233=(
BOUNDED_CURVE()
B_SPLINE_CURVE(2,(#9666,#9667,#9668),.UNSPECIFIED.,.F.,.F.)
B_SPLINE_CURVE_WITH_KNOTS((3,3),(0.140651836354967,0.670383167684795),
 .UNSPECIFIED.)
CURVE()
GEOMETRIC_REPRESENTATION_ITEM()
RATIONAL_B_SPLINE_CURVE((1.11602540378444,1.28867513459481,1.11602540378444))
REPRESENTATION_ITEM('')
);
#234=(
BOUNDED_CURVE()
B_SPLINE_CURVE(2,(#9670,#9671,#9672),.UNSPECIFIED.,.F.,.F.)
B_SPLINE_CURVE_WITH_KNOTS((3,3),(0.140651836354967,0.670383167684795),
 .UNSPECIFIED.)
CURVE()
GEOMETRIC_REPRESENTATION_ITEM()
RATIONAL_B_SPLINE_CURVE((1.11602540378444,1.28867513459481,1.11602540378444))
REPRESENTATION_ITEM('')
);
#235=(
BOUNDED_CURVE()
B_SPLINE_CURVE(2,(#9677,#9678,#9679),.UNSPECIFIED.,.F.,.F.)
B_SPLINE_CURVE_WITH_KNOTS((3,3),(0.140651836354967,0.670383167684795),
 .UNSPECIFIED.)
CURVE()
GEOMETRIC_REPRESENTATION_ITEM()
RATIONAL_B_SPLINE_CURVE((1.11602540378444,1.28867513459481,1.11602540378444))
REPRESENTATION_ITEM('')
);
#236=(
BOUNDED_CURVE()
B_SPLINE_CURVE(2,(#9681,#9682,#9683),.UNSPECIFIED.,.F.,.F.)
B_SPLINE_CURVE_WITH_KNOTS((3,3),(0.140651836354967,0.670383167684795),
 .UNSPECIFIED.)
CURVE()
GEOMETRIC_REPRESENTATION_ITEM()
RATIONAL_B_SPLINE_CURVE((1.11602540378444,1.28867513459481,1.11602540378444))
REPRESENTATION_ITEM('')
);
#237=(
BOUNDED_CURVE()
B_SPLINE_CURVE(2,(#9685,#9686,#9687),.UNSPECIFIED.,.F.,.F.)
B_SPLINE_CURVE_WITH_KNOTS((3,3),(0.140651836354967,0.670383167684795),
 .UNSPECIFIED.)
CURVE()
GEOMETRIC_REPRESENTATION_ITEM()
RATIONAL_B_SPLINE_CURVE((1.11602540378444,1.28867513459481,1.11602540378444))
REPRESENTATION_ITEM('')
);
#238=(
BOUNDED_CURVE()
B_SPLINE_CURVE(2,(#9688,#9689,#9690),.UNSPECIFIED.,.F.,.F.)
B_SPLINE_CURVE_WITH_KNOTS((3,3),(0.140651836354967,0.670383167684795),
 .UNSPECIFIED.)
CURVE()
GEOMETRIC_REPRESENTATION_ITEM()
RATIONAL_B_SPLINE_CURVE((1.11602540378444,1.28867513459481,1.11602540378444))
REPRESENTATION_ITEM('')
);
#239=(
BOUNDED_CURVE()
B_SPLINE_CURVE(2,(#9697,#9698,#9699),.UNSPECIFIED.,.F.,.F.)
B_SPLINE_CURVE_WITH_KNOTS((3,3),(0.140651836354967,0.670383167684795),
 .UNSPECIFIED.)
CURVE()
GEOMETRIC_REPRESENTATION_ITEM()
RATIONAL_B_SPLINE_CURVE((1.11602540378444,1.28867513459481,1.11602540378444))
REPRESENTATION_ITEM('')
);
#240=(
BOUNDED_CURVE()
B_SPLINE_CURVE(2,(#9701,#9702,#9703),.UNSPECIFIED.,.F.,.F.)
B_SPLINE_CURVE_WITH_KNOTS((3,3),(0.140651836354967,0.670383167684796),
 .UNSPECIFIED.)
CURVE()
GEOMETRIC_REPRESENTATION_ITEM()
RATIONAL_B_SPLINE_CURVE((1.11602540378444,1.28867513459481,1.11602540378444))
REPRESENTATION_ITEM('')
);
#241=(
BOUNDED_CURVE()
B_SPLINE_CURVE(2,(#9705,#9706,#9707),.UNSPECIFIED.,.F.,.F.)
B_SPLINE_CURVE_WITH_KNOTS((3,3),(0.140651836354967,0.670383167684795),
 .UNSPECIFIED.)
CURVE()
GEOMETRIC_REPRESENTATION_ITEM()
RATIONAL_B_SPLINE_CURVE((1.11602540378444,1.28867513459481,1.11602540378444))
REPRESENTATION_ITEM('')
);
#242=(
BOUNDED_CURVE()
B_SPLINE_CURVE(2,(#9709,#9710,#9711),.UNSPECIFIED.,.F.,.F.)
B_SPLINE_CURVE_WITH_KNOTS((3,3),(0.140651836354967,0.670383167684795),
 .UNSPECIFIED.)
CURVE()
GEOMETRIC_REPRESENTATION_ITEM()
RATIONAL_B_SPLINE_CURVE((1.11602540378444,1.28867513459482,1.11602540378444))
REPRESENTATION_ITEM('')
);
#243=(
BOUNDED_CURVE()
B_SPLINE_CURVE(2,(#9713,#9714,#9715),.UNSPECIFIED.,.F.,.F.)
B_SPLINE_CURVE_WITH_KNOTS((3,3),(0.140651836354967,0.670383167684795),
 .UNSPECIFIED.)
CURVE()
GEOMETRIC_REPRESENTATION_ITEM()
RATIONAL_B_SPLINE_CURVE((1.11602540378444,1.28867513459481,1.11602540378444))
REPRESENTATION_ITEM('')
);
#244=(
BOUNDED_CURVE()
B_SPLINE_CURVE(2,(#9716,#9717,#9718),.UNSPECIFIED.,.F.,.F.)
B_SPLINE_CURVE_WITH_KNOTS((3,3),(0.140651836354967,0.670383167684795),
 .UNSPECIFIED.)
CURVE()
GEOMETRIC_REPRESENTATION_ITEM()
RATIONAL_B_SPLINE_CURVE((1.11602540378444,1.28867513459481,1.11602540378444))
REPRESENTATION_ITEM('')
);
#245=(
BOUNDED_CURVE()
B_SPLINE_CURVE(2,(#10055,#10056,#10057),.UNSPECIFIED.,.F.,.F.)
B_SPLINE_CURVE_WITH_KNOTS((3,3),(0.144988513094728,0.791574906712449),
 .UNSPECIFIED.)
CURVE()
GEOMETRIC_REPRESENTATION_ITEM()
RATIONAL_B_SPLINE_CURVE((1.09282032302755,1.26188021535082,1.09282032302931))
REPRESENTATION_ITEM('')
);
#246=(
BOUNDED_CURVE()
B_SPLINE_CURVE(2,(#10059,#10060,#10061),.UNSPECIFIED.,.F.,.F.)
B_SPLINE_CURVE_WITH_KNOTS((3,3),(0.144988513094728,0.791574906712449),
 .UNSPECIFIED.)
CURVE()
GEOMETRIC_REPRESENTATION_ITEM()
RATIONAL_B_SPLINE_CURVE((1.09282032302755,1.26188021535082,1.09282032302931))
REPRESENTATION_ITEM('')
);
#247=(
BOUNDED_CURVE()
B_SPLINE_CURVE(2,(#10063,#10064,#10065),.UNSPECIFIED.,.F.,.F.)
B_SPLINE_CURVE_WITH_KNOTS((3,3),(0.144988513094728,0.791574906712449),
 .UNSPECIFIED.)
CURVE()
GEOMETRIC_REPRESENTATION_ITEM()
RATIONAL_B_SPLINE_CURVE((1.09282032302755,1.26188021535082,1.09282032302931))
REPRESENTATION_ITEM('')
);
#248=(
BOUNDED_CURVE()
B_SPLINE_CURVE(2,(#10067,#10068,#10069),.UNSPECIFIED.,.F.,.F.)
B_SPLINE_CURVE_WITH_KNOTS((3,3),(0.144988513094728,0.791574906712449),
 .UNSPECIFIED.)
CURVE()
GEOMETRIC_REPRESENTATION_ITEM()
RATIONAL_B_SPLINE_CURVE((1.09282032302755,1.26188021535082,1.09282032302931))
REPRESENTATION_ITEM('')
);
#249=(
BOUNDED_CURVE()
B_SPLINE_CURVE(2,(#10071,#10072,#10073),.UNSPECIFIED.,.F.,.F.)
B_SPLINE_CURVE_WITH_KNOTS((3,3),(0.144988513094728,0.791574906712449),
 .UNSPECIFIED.)
CURVE()
GEOMETRIC_REPRESENTATION_ITEM()
RATIONAL_B_SPLINE_CURVE((1.09282032302755,1.26188021535082,1.09282032302931))
REPRESENTATION_ITEM('')
);
#250=(
BOUNDED_CURVE()
B_SPLINE_CURVE(2,(#10074,#10075,#10076),.UNSPECIFIED.,.F.,.F.)
B_SPLINE_CURVE_WITH_KNOTS((3,3),(0.144988513094727,0.791574906712449),
 .UNSPECIFIED.)
CURVE()
GEOMETRIC_REPRESENTATION_ITEM()
RATIONAL_B_SPLINE_CURVE((1.09282032302755,1.26188021535082,1.09282032302931))
REPRESENTATION_ITEM('')
);
#251=ORIENTED_CLOSED_SHELL('',*,#5896,.F.);
#252=ORIENTED_CLOSED_SHELL('',*,#5903,.F.);
#253=ORIENTED_CLOSED_SHELL('',*,#5913,.F.);
#254=BREP_WITH_VOIDS('Body1',#5897,(#251));
#255=BREP_WITH_VOIDS('Body1',#5902,(#252));
#256=BREP_WITH_VOIDS('Body1',#5914,(#253));
#257=TOROIDAL_SURFACE('',#6508,0.5,0.1);
#258=SPHERICAL_SURFACE('',#6417,1.6);
#259=SPHERICAL_SURFACE('',#6460,1.6);
#260=SPHERICAL_SURFACE('',#6555,1.5);
#261=SPHERICAL_SURFACE('',#6691,0.513);
#262=SPHERICAL_SURFACE('',#6705,0.825);
#263=SPHERICAL_SURFACE('',#6828,1.5);
#264=CONICAL_SURFACE('',#6349,0.205,0.0748598477107669);
#265=CONICAL_SURFACE('',#6355,0.205,0.0748598477107669);
#266=CONICAL_SURFACE('',#6361,0.205,0.0748598477107669);
#267=CONICAL_SURFACE('',#6582,0.4,0.785398163397448);
#268=CONICAL_SURFACE('',#6586,0.41,0.785398163397448);
#269=CONICAL_SURFACE('',#6590,0.26,0.463647609000806);
#270=CONICAL_SURFACE('',#6594,0.275,0.785398163397449);
#271=CONICAL_SURFACE('',#6605,0.47094010767585,1.0471975511966);
#272=CONICAL_SURFACE('',#6607,0.47094010767585,1.0471975511966);
#273=CONICAL_SURFACE('',#6636,1.025,0.785398163397448);
#274=CONICAL_SURFACE('',#6639,1.025,0.785398163397448);
#275=CONICAL_SURFACE('',#6656,0.325,0.785398163397448);
#276=CONICAL_SURFACE('',#6660,0.335,0.785398163397448);
#277=CONICAL_SURFACE('',#6664,0.21,0.463647609000806);
#278=CONICAL_SURFACE('',#6668,0.18,0.785398163397448);
#279=CONICAL_SURFACE('',#6741,0.645,0.785398163397448);
#280=CONICAL_SURFACE('',#6744,0.645,0.785398163397448);
#281=CONICAL_SURFACE('',#6753,0.27,0.785398163397448);
#282=CONICAL_SURFACE('',#6756,0.576175134594813,1.0471975511966);
#283=CONICAL_SURFACE('',#6905,0.325,0.785398163397448);
#284=CONICAL_SURFACE('',#6909,0.335,0.785398163397448);
#285=CONICAL_SURFACE('',#6913,0.21,0.463647609000806);
#286=SHAPE_REPRESENTATION_RELATIONSHIP('SRR','None',#10643,#315);
#287=SHAPE_REPRESENTATION_RELATIONSHIP('SRR','None',#10644,#316);
#288=SHAPE_REPRESENTATION_RELATIONSHIP('SRR','None',#10645,#317);
#289=SHAPE_REPRESENTATION_RELATIONSHIP('SRR','None',#10646,#318);
#290=SHAPE_REPRESENTATION_RELATIONSHIP('SRR','None',#10647,#319);
#291=SHAPE_REPRESENTATION_RELATIONSHIP('SRR','None',#10648,#320);
#292=SHAPE_REPRESENTATION_RELATIONSHIP('SRR','None',#10649,#321);
#293=SHAPE_REPRESENTATION_RELATIONSHIP('SRR','None',#10650,#322);
#294=SHAPE_REPRESENTATION_RELATIONSHIP('SRR','None',#10651,#323);
#295=SHAPE_REPRESENTATION_RELATIONSHIP('SRR','None',#10652,#324);
#296=SHAPE_REPRESENTATION_RELATIONSHIP('SRR','None',#10653,#325);
#297=SHAPE_REPRESENTATION_RELATIONSHIP('SRR','None',#10654,#326);
#298=SHAPE_REPRESENTATION_RELATIONSHIP('SRR','None',#10655,#327);
#299=SHAPE_REPRESENTATION_RELATIONSHIP('SRR','None',#10656,#328);
#300=SHAPE_REPRESENTATION_RELATIONSHIP('SRR','None',#10657,#329);
#301=SHAPE_REPRESENTATION_RELATIONSHIP('SRR','None',#10658,#330);
#302=SHAPE_REPRESENTATION_RELATIONSHIP('SRR','None',#10659,#331);
#303=SHAPE_REPRESENTATION_RELATIONSHIP('SRR','None',#10660,#332);
#304=SHAPE_REPRESENTATION_RELATIONSHIP('SRR','None',#10661,#333);
#305=SHAPE_REPRESENTATION_RELATIONSHIP('SRR','None',#10662,#334);
#306=SHAPE_REPRESENTATION_RELATIONSHIP('SRR','None',#10663,#335);
#307=SHAPE_REPRESENTATION_RELATIONSHIP('SRR','None',#10664,#336);
#308=SHAPE_REPRESENTATION_RELATIONSHIP('SRR','None',#10665,#337);
#309=SHAPE_REPRESENTATION_RELATIONSHIP('SRR','None',#10667,#338);
#310=SHAPE_REPRESENTATION_RELATIONSHIP('SRR','None',#10668,#339);
#311=SHAPE_REPRESENTATION_RELATIONSHIP('SRR','None',#10669,#340);
#312=SHAPE_REPRESENTATION_RELATIONSHIP('SRR','None',#10670,#341);
#313=SHAPE_REPRESENTATION_RELATIONSHIP('SRR','None',#10671,#342);
#314=SHAPE_REPRESENTATION_RELATIONSHIP('SRR','None',#10672,#343);
#315=ADVANCED_BREP_SHAPE_REPRESENTATION('',(#373),#10487);
#316=ADVANCED_BREP_SHAPE_REPRESENTATION('',(#374),#10488);
#317=ADVANCED_BREP_SHAPE_REPRESENTATION('',(#375),#10489);
#318=ADVANCED_BREP_SHAPE_REPRESENTATION('',(#376),#10490);
#319=ADVANCED_BREP_SHAPE_REPRESENTATION('',(#377),#10491);
#320=ADVANCED_BREP_SHAPE_REPRESENTATION('',(#378),#10492);
#321=ADVANCED_BREP_SHAPE_REPRESENTATION('',(#379),#10493);
#322=ADVANCED_BREP_SHAPE_REPRESENTATION('',(#380),#10494);
#323=ADVANCED_BREP_SHAPE_REPRESENTATION('',(#381),#10495);
#324=ADVANCED_BREP_SHAPE_REPRESENTATION('',(#382),#10496);
#325=ADVANCED_BREP_SHAPE_REPRESENTATION('',(#383),#10497);
#326=ADVANCED_BREP_SHAPE_REPRESENTATION('',(#384),#10498);
#327=ADVANCED_BREP_SHAPE_REPRESENTATION('',(#385),#10499);
#328=ADVANCED_BREP_SHAPE_REPRESENTATION('',(#254),#10500);
#329=ADVANCED_BREP_SHAPE_REPRESENTATION('',(#386),#10501);
#330=ADVANCED_BREP_SHAPE_REPRESENTATION('',(#387),#10502);
#331=ADVANCED_BREP_SHAPE_REPRESENTATION('',(#388),#10503);
#332=ADVANCED_BREP_SHAPE_REPRESENTATION('',(#389),#10504);
#333=ADVANCED_BREP_SHAPE_REPRESENTATION('',(#255),#10505);
#334=ADVANCED_BREP_SHAPE_REPRESENTATION('',(#390),#10506);
#335=ADVANCED_BREP_SHAPE_REPRESENTATION('',(#391),#10507);
#336=ADVANCED_BREP_SHAPE_REPRESENTATION('',(#392),#10508);
#337=ADVANCED_BREP_SHAPE_REPRESENTATION('',(#393),#10509);
#338=ADVANCED_BREP_SHAPE_REPRESENTATION('',(#394),#10511);
#339=ADVANCED_BREP_SHAPE_REPRESENTATION('',(#395),#10512);
#340=ADVANCED_BREP_SHAPE_REPRESENTATION('',(#396),#10513);
#341=ADVANCED_BREP_SHAPE_REPRESENTATION('',(#397),#10514);
#342=ADVANCED_BREP_SHAPE_REPRESENTATION('',(#398),#10515);
#343=ADVANCED_BREP_SHAPE_REPRESENTATION('',(#256),#10516);
#344=STYLED_ITEM('',(#10860),#373);
#345=STYLED_ITEM('',(#10860),#374);
#346=STYLED_ITEM('',(#10853),#375);
#347=STYLED_ITEM('',(#10881),#376);
#348=STYLED_ITEM('',(#10860),#377);
#349=STYLED_ITEM('',(#10853),#378);
#350=STYLED_ITEM('',(#10853),#379);
#351=STYLED_ITEM('',(#10853),#380);
#352=STYLED_ITEM('',(#10867),#381);
#353=STYLED_ITEM('',(#10867),#382);
#354=STYLED_ITEM('',(#10860),#383);
#355=STYLED_ITEM('',(#10860),#384);
#356=STYLED_ITEM('',(#10860),#385);
#357=STYLED_ITEM('',(#10881),#254);
#358=STYLED_ITEM('',(#10881),#386);
#359=STYLED_ITEM('',(#10881),#387);
#360=STYLED_ITEM('',(#10860),#388);
#361=STYLED_ITEM('',(#10867),#389);
#362=STYLED_ITEM('',(#10881),#255);
#363=STYLED_ITEM('',(#10874),#390);
#364=STYLED_ITEM('',(#10888),#391);
#365=STYLED_ITEM('',(#10867),#392);
#366=STYLED_ITEM('',(#10881),#393);
#367=STYLED_ITEM('',(#10860),#394);
#368=STYLED_ITEM('',(#10867),#395);
#369=STYLED_ITEM('',(#10888),#396);
#370=STYLED_ITEM('',(#10867),#397);
#371=STYLED_ITEM('',(#10881),#398);
#372=STYLED_ITEM('',(#10881),#256);
#373=MANIFOLD_SOLID_BREP('Body1',#5883);
#374=MANIFOLD_SOLID_BREP('Body1',#5884);
#375=MANIFOLD_SOLID_BREP('Body1',#5885);
#376=MANIFOLD_SOLID_BREP('Body1',#5886);
#377=MANIFOLD_SOLID_BREP('Body1',#5887);
#378=MANIFOLD_SOLID_BREP('Body1',#5888);
#379=MANIFOLD_SOLID_BREP('Body1',#5889);
#380=MANIFOLD_SOLID_BREP('Body1',#5890);
#381=MANIFOLD_SOLID_BREP('Body1',#5891);
#382=MANIFOLD_SOLID_BREP('Body1',#5892);
#383=MANIFOLD_SOLID_BREP('Body1',#5893);
#384=MANIFOLD_SOLID_BREP('Body1',#5894);
#385=MANIFOLD_SOLID_BREP('Body1',#5895);
#386=MANIFOLD_SOLID_BREP('Body1',#5898);
#387=MANIFOLD_SOLID_BREP('Body1',#5899);
#388=MANIFOLD_SOLID_BREP('Body1',#5900);
#389=MANIFOLD_SOLID_BREP('Body1',#5901);
#390=MANIFOLD_SOLID_BREP('Body1',#5904);
#391=MANIFOLD_SOLID_BREP('Body1',#5905);
#392=MANIFOLD_SOLID_BREP('Body1',#5906);
#393=MANIFOLD_SOLID_BREP('Body1',#5907);
#394=MANIFOLD_SOLID_BREP('Body1',#5908);
#395=MANIFOLD_SOLID_BREP('Body1',#5909);
#396=MANIFOLD_SOLID_BREP('Body1',#5910);
#397=MANIFOLD_SOLID_BREP('Body1',#5911);
#398=MANIFOLD_SOLID_BREP('Body1',#5912);
#399=FACE_BOUND('',#1112,.T.);
#400=FACE_BOUND('',#1115,.T.);
#401=FACE_BOUND('',#1119,.T.);
#402=FACE_BOUND('',#1121,.T.);
#403=FACE_BOUND('',#1124,.T.);
#404=FACE_BOUND('',#1127,.T.);
#405=FACE_BOUND('',#1131,.T.);
#406=FACE_BOUND('',#1133,.T.);
#407=FACE_BOUND('',#1141,.T.);
#408=FACE_BOUND('',#1146,.T.);
#409=FACE_BOUND('',#1148,.T.);
#410=FACE_BOUND('',#1155,.T.);
#411=FACE_BOUND('',#1161,.T.);
#412=FACE_BOUND('',#1163,.T.);
#413=FACE_BOUND('',#1170,.T.);
#414=FACE_BOUND('',#1174,.T.);
#415=FACE_BOUND('',#1175,.T.);
#416=FACE_BOUND('',#1176,.T.);
#417=FACE_BOUND('',#1177,.T.);
#418=FACE_BOUND('',#1178,.T.);
#419=FACE_BOUND('',#1179,.T.);
#420=FACE_BOUND('',#1180,.T.);
#421=FACE_BOUND('',#1183,.T.);
#422=FACE_BOUND('',#1184,.T.);
#423=FACE_BOUND('',#1185,.T.);
#424=FACE_BOUND('',#1186,.T.);
#425=FACE_BOUND('',#1187,.T.);
#426=FACE_BOUND('',#1198,.T.);
#427=FACE_BOUND('',#1200,.T.);
#428=FACE_BOUND('',#1202,.T.);
#429=FACE_BOUND('',#1205,.T.);
#430=FACE_BOUND('',#1209,.T.);
#431=FACE_BOUND('',#1213,.T.);
#432=FACE_BOUND('',#1217,.T.);
#433=FACE_BOUND('',#1225,.T.);
#434=FACE_BOUND('',#1228,.T.);
#435=FACE_BOUND('',#1240,.T.);
#436=FACE_BOUND('',#1241,.T.);
#437=FACE_BOUND('',#1245,.T.);
#438=FACE_BOUND('',#1247,.T.);
#439=FACE_BOUND('',#1249,.T.);
#440=FACE_BOUND('',#1251,.T.);
#441=FACE_BOUND('',#1252,.T.);
#442=FACE_BOUND('',#1253,.T.);
#443=FACE_BOUND('',#1254,.T.);
#444=FACE_BOUND('',#1257,.T.);
#445=FACE_BOUND('',#1258,.T.);
#446=FACE_BOUND('',#1259,.T.);
#447=FACE_BOUND('',#1260,.T.);
#448=FACE_BOUND('',#1261,.T.);
#449=FACE_BOUND('',#1275,.T.);
#450=FACE_BOUND('',#1276,.T.);
#451=FACE_BOUND('',#1280,.T.);
#452=FACE_BOUND('',#1282,.T.);
#453=FACE_BOUND('',#1284,.T.);
#454=FACE_BOUND('',#1286,.T.);
#455=FACE_BOUND('',#1287,.T.);
#456=FACE_BOUND('',#1288,.T.);
#457=FACE_BOUND('',#1289,.T.);
#458=FACE_BOUND('',#1290,.T.);
#459=FACE_BOUND('',#1293,.T.);
#460=FACE_BOUND('',#1294,.T.);
#461=FACE_BOUND('',#1295,.T.);
#462=FACE_BOUND('',#1296,.T.);
#463=FACE_BOUND('',#1308,.T.);
#464=FACE_BOUND('',#1309,.T.);
#465=FACE_BOUND('',#1310,.T.);
#466=FACE_BOUND('',#1311,.T.);
#467=FACE_BOUND('',#1319,.T.);
#468=FACE_BOUND('',#1320,.T.);
#469=FACE_BOUND('',#1321,.T.);
#470=FACE_BOUND('',#1322,.T.);
#471=FACE_BOUND('',#1324,.T.);
#472=FACE_BOUND('',#1327,.T.);
#473=FACE_BOUND('',#1331,.T.);
#474=FACE_BOUND('',#1335,.T.);
#475=FACE_BOUND('',#1339,.T.);
#476=FACE_BOUND('',#1341,.T.);
#477=FACE_BOUND('',#1356,.T.);
#478=FACE_BOUND('',#1357,.T.);
#479=FACE_BOUND('',#1358,.T.);
#480=FACE_BOUND('',#1359,.T.);
#481=FACE_BOUND('',#1360,.T.);
#482=FACE_BOUND('',#1361,.T.);
#483=FACE_BOUND('',#1362,.T.);
#484=FACE_BOUND('',#1364,.T.);
#485=FACE_BOUND('',#1365,.T.);
#486=FACE_BOUND('',#1366,.T.);
#487=FACE_BOUND('',#1367,.T.);
#488=FACE_BOUND('',#1368,.T.);
#489=FACE_BOUND('',#1370,.T.);
#490=FACE_BOUND('',#1374,.T.);
#491=FACE_BOUND('',#1376,.T.);
#492=FACE_BOUND('',#1386,.T.);
#493=FACE_BOUND('',#1394,.T.);
#494=FACE_BOUND('',#1400,.T.);
#495=FACE_BOUND('',#1403,.T.);
#496=FACE_BOUND('',#1414,.T.);
#497=FACE_BOUND('',#1416,.T.);
#498=FACE_BOUND('',#1418,.T.);
#499=FACE_BOUND('',#1420,.T.);
#500=FACE_BOUND('',#1429,.T.);
#501=FACE_BOUND('',#1434,.T.);
#502=FACE_BOUND('',#1439,.T.);
#503=FACE_BOUND('',#1441,.T.);
#504=FACE_BOUND('',#1447,.T.);
#505=FACE_BOUND('',#1465,.T.);
#506=FACE_BOUND('',#1468,.T.);
#507=FACE_BOUND('',#1472,.T.);
#508=FACE_BOUND('',#1476,.T.);
#509=FACE_BOUND('',#1479,.T.);
#510=FACE_BOUND('',#1481,.T.);
#511=FACE_BOUND('',#1484,.T.);
#512=FACE_BOUND('',#1487,.T.);
#513=FACE_BOUND('',#1489,.T.);
#514=FACE_BOUND('',#1498,.T.);
#515=FACE_BOUND('',#1503,.T.);
#516=FACE_BOUND('',#1517,.T.);
#517=FACE_BOUND('',#1525,.T.);
#518=FACE_BOUND('',#1526,.T.);
#519=FACE_BOUND('',#1538,.T.);
#520=FACE_BOUND('',#1550,.T.);
#521=FACE_BOUND('',#1560,.T.);
#522=FACE_BOUND('',#1562,.T.);
#523=FACE_BOUND('',#1566,.T.);
#524=FACE_BOUND('',#1568,.T.);
#525=FACE_BOUND('',#1589,.T.);
#526=PLANE('',#6241);
#527=PLANE('',#6246);
#528=PLANE('',#6252);
#529=PLANE('',#6253);
#530=PLANE('',#6258);
#531=PLANE('',#6263);
#532=PLANE('',#6269);
#533=PLANE('',#6270);
#534=PLANE('',#6290);
#535=PLANE('',#6294);
#536=PLANE('',#6298);
#537=PLANE('',#6299);
#538=PLANE('',#6300);
#539=PLANE('',#6304);
#540=PLANE('',#6305);
#541=PLANE('',#6306);
#542=PLANE('',#6307);
#543=PLANE('',#6308);
#544=PLANE('',#6312);
#545=PLANE('',#6316);
#546=PLANE('',#6317);
#547=PLANE('',#6318);
#548=PLANE('',#6322);
#549=PLANE('',#6323);
#550=PLANE('',#6324);
#551=PLANE('',#6325);
#552=PLANE('',#6326);
#553=PLANE('',#6327);
#554=PLANE('',#6328);
#555=PLANE('',#6329);
#556=PLANE('',#6330);
#557=PLANE('',#6331);
#558=PLANE('',#6332);
#559=PLANE('',#6337);
#560=PLANE('',#6338);
#561=PLANE('',#6339);
#562=PLANE('',#6340);
#563=PLANE('',#6341);
#564=PLANE('',#6342);
#565=PLANE('',#6343);
#566=PLANE('',#6344);
#567=PLANE('',#6346);
#568=PLANE('',#6351);
#569=PLANE('',#6357);
#570=PLANE('',#6363);
#571=PLANE('',#6369);
#572=PLANE('',#6371);
#573=PLANE('',#6372);
#574=PLANE('',#6373);
#575=PLANE('',#6374);
#576=PLANE('',#6375);
#577=PLANE('',#6376);
#578=PLANE('',#6377);
#579=PLANE('',#6380);
#580=PLANE('',#6385);
#581=PLANE('',#6389);
#582=PLANE('',#6405);
#583=PLANE('',#6407);
#584=PLANE('',#6414);
#585=PLANE('',#6416);
#586=PLANE('',#6419);
#587=PLANE('',#6420);
#588=PLANE('',#6421);
#589=PLANE('',#6422);
#590=PLANE('',#6423);
#591=PLANE('',#6428);
#592=PLANE('',#6432);
#593=PLANE('',#6448);
#594=PLANE('',#6450);
#595=PLANE('',#6457);
#596=PLANE('',#6458);
#597=PLANE('',#6462);
#598=PLANE('',#6463);
#599=PLANE('',#6464);
#600=PLANE('',#6465);
#601=PLANE('',#6466);
#602=PLANE('',#6480);
#603=PLANE('',#6481);
#604=PLANE('',#6482);
#605=PLANE('',#6483);
#606=PLANE('',#6484);
#607=PLANE('',#6486);
#608=PLANE('',#6487);
#609=PLANE('',#6490);
#610=PLANE('',#6491);
#611=PLANE('',#6492);
#612=PLANE('',#6493);
#613=PLANE('',#6495);
#614=PLANE('',#6500);
#615=PLANE('',#6506);
#616=PLANE('',#6515);
#617=PLANE('',#6522);
#618=PLANE('',#6523);
#619=PLANE('',#6528);
#620=PLANE('',#6532);
#621=PLANE('',#6548);
#622=PLANE('',#6549);
#623=PLANE('',#6550);
#624=PLANE('',#6551);
#625=PLANE('',#6552);
#626=PLANE('',#6553);
#627=PLANE('',#6563);
#628=PLANE('',#6564);
#629=PLANE('',#6566);
#630=PLANE('',#6567);
#631=PLANE('',#6568);
#632=PLANE('',#6569);
#633=PLANE('',#6570);
#634=PLANE('',#6571);
#635=PLANE('',#6572);
#636=PLANE('',#6573);
#637=PLANE('',#6574);
#638=PLANE('',#6579);
#639=PLANE('',#6580);
#640=PLANE('',#6588);
#641=PLANE('',#6599);
#642=PLANE('',#6603);
#643=PLANE('',#6609);
#644=PLANE('',#6610);
#645=PLANE('',#6611);
#646=PLANE('',#6615);
#647=PLANE('',#6616);
#648=PLANE('',#6617);
#649=PLANE('',#6618);
#650=PLANE('',#6619);
#651=PLANE('',#6621);
#652=PLANE('',#6623);
#653=PLANE('',#6625);
#654=PLANE('',#6626);
#655=PLANE('',#6627);
#656=PLANE('',#6628);
#657=PLANE('',#6629);
#658=PLANE('',#6630);
#659=PLANE('',#6633);
#660=PLANE('',#6641);
#661=PLANE('',#6651);
#662=PLANE('',#6652);
#663=PLANE('',#6654);
#664=PLANE('',#6662);
#665=PLANE('',#6670);
#666=PLANE('',#6671);
#667=PLANE('',#6672);
#668=PLANE('',#6673);
#669=PLANE('',#6674);
#670=PLANE('',#6675);
#671=PLANE('',#6676);
#672=PLANE('',#6677);
#673=PLANE('',#6678);
#674=PLANE('',#6683);
#675=PLANE('',#6684);
#676=PLANE('',#6697);
#677=PLANE('',#6704);
#678=PLANE('',#6713);
#679=PLANE('',#6717);
#680=PLANE('',#6718);
#681=PLANE('',#6723);
#682=PLANE('',#6726);
#683=PLANE('',#6728);
#684=PLANE('',#6730);
#685=PLANE('',#6731);
#686=PLANE('',#6732);
#687=PLANE('',#6733);
#688=PLANE('',#6734);
#689=PLANE('',#6735);
#690=PLANE('',#6738);
#691=PLANE('',#6746);
#692=PLANE('',#6755);
#693=PLANE('',#6758);
#694=PLANE('',#6759);
#695=PLANE('',#6760);
#696=PLANE('',#6761);
#697=PLANE('',#6762);
#698=PLANE('',#6763);
#699=PLANE('',#6764);
#700=PLANE('',#6765);
#701=PLANE('',#6815);
#702=PLANE('',#6817);
#703=PLANE('',#6820);
#704=PLANE('',#6822);
#705=PLANE('',#6824);
#706=PLANE('',#6834);
#707=PLANE('',#6835);
#708=PLANE('',#6837);
#709=PLANE('',#6839);
#710=PLANE('',#6841);
#711=PLANE('',#6843);
#712=PLANE('',#6844);
#713=PLANE('',#6845);
#714=PLANE('',#6846);
#715=PLANE('',#6847);
#716=PLANE('',#6848);
#717=PLANE('',#6850);
#718=PLANE('',#6853);
#719=PLANE('',#6855);
#720=PLANE('',#6857);
#721=PLANE('',#6858);
#722=PLANE('',#6859);
#723=PLANE('',#6860);
#724=PLANE('',#6861);
#725=PLANE('',#6864);
#726=PLANE('',#6866);
#727=PLANE('',#6867);
#728=PLANE('',#6868);
#729=PLANE('',#6869);
#730=PLANE('',#6870);
#731=PLANE('',#6871);
#732=PLANE('',#6872);
#733=PLANE('',#6873);
#734=PLANE('',#6874);
#735=PLANE('',#6875);
#736=PLANE('',#6883);
#737=PLANE('',#6884);
#738=PLANE('',#6886);
#739=PLANE('',#6887);
#740=PLANE('',#6888);
#741=PLANE('',#6889);
#742=PLANE('',#6890);
#743=PLANE('',#6891);
#744=PLANE('',#6893);
#745=PLANE('',#6894);
#746=PLANE('',#6895);
#747=PLANE('',#6896);
#748=PLANE('',#6897);
#749=PLANE('',#6898);
#750=PLANE('',#6899);
#751=PLANE('',#6900);
#752=PLANE('',#6901);
#753=PLANE('',#6903);
#754=PLANE('',#6911);
#755=FACE_OUTER_BOUND('',#1110,.T.);
#756=FACE_OUTER_BOUND('',#1111,.T.);
#757=FACE_OUTER_BOUND('',#1113,.T.);
#758=FACE_OUTER_BOUND('',#1114,.T.);
#759=FACE_OUTER_BOUND('',#1116,.T.);
#760=FACE_OUTER_BOUND('',#1117,.T.);
#761=FACE_OUTER_BOUND('',#1118,.T.);
#762=FACE_OUTER_BOUND('',#1120,.T.);
#763=FACE_OUTER_BOUND('',#1122,.T.);
#764=FACE_OUTER_BOUND('',#1123,.T.);
#765=FACE_OUTER_BOUND('',#1125,.T.);
#766=FACE_OUTER_BOUND('',#1126,.T.);
#767=FACE_OUTER_BOUND('',#1128,.T.);
#768=FACE_OUTER_BOUND('',#1129,.T.);
#769=FACE_OUTER_BOUND('',#1130,.T.);
#770=FACE_OUTER_BOUND('',#1132,.T.);
#771=FACE_OUTER_BOUND('',#1134,.T.);
#772=FACE_OUTER_BOUND('',#1135,.T.);
#773=FACE_OUTER_BOUND('',#1136,.T.);
#774=FACE_OUTER_BOUND('',#1137,.T.);
#775=FACE_OUTER_BOUND('',#1138,.T.);
#776=FACE_OUTER_BOUND('',#1139,.T.);
#777=FACE_OUTER_BOUND('',#1140,.T.);
#778=FACE_OUTER_BOUND('',#1142,.T.);
#779=FACE_OUTER_BOUND('',#1143,.T.);
#780=FACE_OUTER_BOUND('',#1144,.T.);
#781=FACE_OUTER_BOUND('',#1145,.T.);
#782=FACE_OUTER_BOUND('',#1147,.T.);
#783=FACE_OUTER_BOUND('',#1149,.T.);
#784=FACE_OUTER_BOUND('',#1150,.T.);
#785=FACE_OUTER_BOUND('',#1151,.T.);
#786=FACE_OUTER_BOUND('',#1152,.T.);
#787=FACE_OUTER_BOUND('',#1153,.T.);
#788=FACE_OUTER_BOUND('',#1154,.T.);
#789=FACE_OUTER_BOUND('',#1156,.T.);
#790=FACE_OUTER_BOUND('',#1157,.T.);
#791=FACE_OUTER_BOUND('',#1158,.T.);
#792=FACE_OUTER_BOUND('',#1159,.T.);
#793=FACE_OUTER_BOUND('',#1160,.T.);
#794=FACE_OUTER_BOUND('',#1162,.T.);
#795=FACE_OUTER_BOUND('',#1164,.T.);
#796=FACE_OUTER_BOUND('',#1165,.T.);
#797=FACE_OUTER_BOUND('',#1166,.T.);
#798=FACE_OUTER_BOUND('',#1167,.T.);
#799=FACE_OUTER_BOUND('',#1168,.T.);
#800=FACE_OUTER_BOUND('',#1169,.T.);
#801=FACE_OUTER_BOUND('',#1171,.T.);
#802=FACE_OUTER_BOUND('',#1172,.T.);
#803=FACE_OUTER_BOUND('',#1173,.T.);
#804=FACE_OUTER_BOUND('',#1181,.T.);
#805=FACE_OUTER_BOUND('',#1182,.T.);
#806=FACE_OUTER_BOUND('',#1188,.T.);
#807=FACE_OUTER_BOUND('',#1189,.T.);
#808=FACE_OUTER_BOUND('',#1190,.T.);
#809=FACE_OUTER_BOUND('',#1191,.T.);
#810=FACE_OUTER_BOUND('',#1192,.T.);
#811=FACE_OUTER_BOUND('',#1193,.T.);
#812=FACE_OUTER_BOUND('',#1194,.T.);
#813=FACE_OUTER_BOUND('',#1195,.T.);
#814=FACE_OUTER_BOUND('',#1196,.T.);
#815=FACE_OUTER_BOUND('',#1197,.T.);
#816=FACE_OUTER_BOUND('',#1199,.T.);
#817=FACE_OUTER_BOUND('',#1201,.T.);
#818=FACE_OUTER_BOUND('',#1203,.T.);
#819=FACE_OUTER_BOUND('',#1204,.T.);
#820=FACE_OUTER_BOUND('',#1206,.T.);
#821=FACE_OUTER_BOUND('',#1207,.T.);
#822=FACE_OUTER_BOUND('',#1208,.T.);
#823=FACE_OUTER_BOUND('',#1210,.T.);
#824=FACE_OUTER_BOUND('',#1211,.T.);
#825=FACE_OUTER_BOUND('',#1212,.T.);
#826=FACE_OUTER_BOUND('',#1214,.T.);
#827=FACE_OUTER_BOUND('',#1215,.T.);
#828=FACE_OUTER_BOUND('',#1216,.T.);
#829=FACE_OUTER_BOUND('',#1218,.T.);
#830=FACE_OUTER_BOUND('',#1219,.T.);
#831=FACE_OUTER_BOUND('',#1220,.T.);
#832=FACE_OUTER_BOUND('',#1221,.T.);
#833=FACE_OUTER_BOUND('',#1222,.T.);
#834=FACE_OUTER_BOUND('',#1223,.T.);
#835=FACE_OUTER_BOUND('',#1224,.T.);
#836=FACE_OUTER_BOUND('',#1226,.T.);
#837=FACE_OUTER_BOUND('',#1227,.T.);
#838=FACE_OUTER_BOUND('',#1229,.T.);
#839=FACE_OUTER_BOUND('',#1230,.T.);
#840=FACE_OUTER_BOUND('',#1231,.T.);
#841=FACE_OUTER_BOUND('',#1232,.T.);
#842=FACE_OUTER_BOUND('',#1233,.T.);
#843=FACE_OUTER_BOUND('',#1234,.T.);
#844=FACE_OUTER_BOUND('',#1235,.T.);
#845=FACE_OUTER_BOUND('',#1236,.T.);
#846=FACE_OUTER_BOUND('',#1237,.T.);
#847=FACE_OUTER_BOUND('',#1238,.T.);
#848=FACE_OUTER_BOUND('',#1239,.T.);
#849=FACE_OUTER_BOUND('',#1242,.T.);
#850=FACE_OUTER_BOUND('',#1243,.T.);
#851=FACE_OUTER_BOUND('',#1244,.T.);
#852=FACE_OUTER_BOUND('',#1246,.T.);
#853=FACE_OUTER_BOUND('',#1248,.T.);
#854=FACE_OUTER_BOUND('',#1250,.T.);
#855=FACE_OUTER_BOUND('',#1255,.T.);
#856=FACE_OUTER_BOUND('',#1256,.T.);
#857=FACE_OUTER_BOUND('',#1262,.T.);
#858=FACE_OUTER_BOUND('',#1263,.T.);
#859=FACE_OUTER_BOUND('',#1264,.T.);
#860=FACE_OUTER_BOUND('',#1265,.T.);
#861=FACE_OUTER_BOUND('',#1266,.T.);
#862=FACE_OUTER_BOUND('',#1267,.T.);
#863=FACE_OUTER_BOUND('',#1268,.T.);
#864=FACE_OUTER_BOUND('',#1269,.T.);
#865=FACE_OUTER_BOUND('',#1270,.T.);
#866=FACE_OUTER_BOUND('',#1271,.T.);
#867=FACE_OUTER_BOUND('',#1272,.T.);
#868=FACE_OUTER_BOUND('',#1273,.T.);
#869=FACE_OUTER_BOUND('',#1274,.T.);
#870=FACE_OUTER_BOUND('',#1277,.T.);
#871=FACE_OUTER_BOUND('',#1278,.T.);
#872=FACE_OUTER_BOUND('',#1279,.T.);
#873=FACE_OUTER_BOUND('',#1281,.T.);
#874=FACE_OUTER_BOUND('',#1283,.T.);
#875=FACE_OUTER_BOUND('',#1285,.T.);
#876=FACE_OUTER_BOUND('',#1291,.T.);
#877=FACE_OUTER_BOUND('',#1292,.T.);
#878=FACE_OUTER_BOUND('',#1297,.T.);
#879=FACE_OUTER_BOUND('',#1298,.T.);
#880=FACE_OUTER_BOUND('',#1299,.T.);
#881=FACE_OUTER_BOUND('',#1300,.T.);
#882=FACE_OUTER_BOUND('',#1301,.T.);
#883=FACE_OUTER_BOUND('',#1302,.T.);
#884=FACE_OUTER_BOUND('',#1303,.T.);
#885=FACE_OUTER_BOUND('',#1304,.T.);
#886=FACE_OUTER_BOUND('',#1305,.T.);
#887=FACE_OUTER_BOUND('',#1306,.T.);
#888=FACE_OUTER_BOUND('',#1307,.T.);
#889=FACE_OUTER_BOUND('',#1312,.T.);
#890=FACE_OUTER_BOUND('',#1313,.T.);
#891=FACE_OUTER_BOUND('',#1314,.T.);
#892=FACE_OUTER_BOUND('',#1315,.T.);
#893=FACE_OUTER_BOUND('',#1316,.T.);
#894=FACE_OUTER_BOUND('',#1317,.T.);
#895=FACE_OUTER_BOUND('',#1318,.T.);
#896=FACE_OUTER_BOUND('',#1323,.T.);
#897=FACE_OUTER_BOUND('',#1325,.T.);
#898=FACE_OUTER_BOUND('',#1326,.T.);
#899=FACE_OUTER_BOUND('',#1328,.T.);
#900=FACE_OUTER_BOUND('',#1329,.T.);
#901=FACE_OUTER_BOUND('',#1330,.T.);
#902=FACE_OUTER_BOUND('',#1332,.T.);
#903=FACE_OUTER_BOUND('',#1333,.T.);
#904=FACE_OUTER_BOUND('',#1334,.T.);
#905=FACE_OUTER_BOUND('',#1336,.T.);
#906=FACE_OUTER_BOUND('',#1337,.T.);
#907=FACE_OUTER_BOUND('',#1338,.T.);
#908=FACE_OUTER_BOUND('',#1340,.T.);
#909=FACE_OUTER_BOUND('',#1342,.T.);
#910=FACE_OUTER_BOUND('',#1343,.T.);
#911=FACE_OUTER_BOUND('',#1344,.T.);
#912=FACE_OUTER_BOUND('',#1345,.T.);
#913=FACE_OUTER_BOUND('',#1346,.T.);
#914=FACE_OUTER_BOUND('',#1347,.T.);
#915=FACE_OUTER_BOUND('',#1348,.T.);
#916=FACE_OUTER_BOUND('',#1349,.T.);
#917=FACE_OUTER_BOUND('',#1350,.T.);
#918=FACE_OUTER_BOUND('',#1351,.T.);
#919=FACE_OUTER_BOUND('',#1352,.T.);
#920=FACE_OUTER_BOUND('',#1353,.T.);
#921=FACE_OUTER_BOUND('',#1354,.T.);
#922=FACE_OUTER_BOUND('',#1355,.T.);
#923=FACE_OUTER_BOUND('',#1363,.T.);
#924=FACE_OUTER_BOUND('',#1369,.T.);
#925=FACE_OUTER_BOUND('',#1371,.T.);
#926=FACE_OUTER_BOUND('',#1372,.T.);
#927=FACE_OUTER_BOUND('',#1373,.T.);
#928=FACE_OUTER_BOUND('',#1375,.T.);
#929=FACE_OUTER_BOUND('',#1377,.T.);
#930=FACE_OUTER_BOUND('',#1378,.T.);
#931=FACE_OUTER_BOUND('',#1379,.T.);
#932=FACE_OUTER_BOUND('',#1380,.T.);
#933=FACE_OUTER_BOUND('',#1381,.T.);
#934=FACE_OUTER_BOUND('',#1382,.T.);
#935=FACE_OUTER_BOUND('',#1383,.T.);
#936=FACE_OUTER_BOUND('',#1384,.T.);
#937=FACE_OUTER_BOUND('',#1385,.T.);
#938=FACE_OUTER_BOUND('',#1387,.T.);
#939=FACE_OUTER_BOUND('',#1388,.T.);
#940=FACE_OUTER_BOUND('',#1389,.T.);
#941=FACE_OUTER_BOUND('',#1390,.T.);
#942=FACE_OUTER_BOUND('',#1391,.T.);
#943=FACE_OUTER_BOUND('',#1392,.T.);
#944=FACE_OUTER_BOUND('',#1393,.T.);
#945=FACE_OUTER_BOUND('',#1395,.T.);
#946=FACE_OUTER_BOUND('',#1396,.T.);
#947=FACE_OUTER_BOUND('',#1397,.T.);
#948=FACE_OUTER_BOUND('',#1398,.T.);
#949=FACE_OUTER_BOUND('',#1399,.T.);
#950=FACE_OUTER_BOUND('',#1401,.T.);
#951=FACE_OUTER_BOUND('',#1402,.T.);
#952=FACE_OUTER_BOUND('',#1404,.T.);
#953=FACE_OUTER_BOUND('',#1405,.T.);
#954=FACE_OUTER_BOUND('',#1406,.T.);
#955=FACE_OUTER_BOUND('',#1407,.T.);
#956=FACE_OUTER_BOUND('',#1408,.T.);
#957=FACE_OUTER_BOUND('',#1409,.T.);
#958=FACE_OUTER_BOUND('',#1410,.T.);
#959=FACE_OUTER_BOUND('',#1411,.T.);
#960=FACE_OUTER_BOUND('',#1412,.T.);
#961=FACE_OUTER_BOUND('',#1413,.T.);
#962=FACE_OUTER_BOUND('',#1415,.T.);
#963=FACE_OUTER_BOUND('',#1417,.T.);
#964=FACE_OUTER_BOUND('',#1419,.T.);
#965=FACE_OUTER_BOUND('',#1421,.T.);
#966=FACE_OUTER_BOUND('',#1422,.T.);
#967=FACE_OUTER_BOUND('',#1423,.T.);
#968=FACE_OUTER_BOUND('',#1424,.T.);
#969=FACE_OUTER_BOUND('',#1425,.T.);
#970=FACE_OUTER_BOUND('',#1426,.T.);
#971=FACE_OUTER_BOUND('',#1427,.T.);
#972=FACE_OUTER_BOUND('',#1428,.T.);
#973=FACE_OUTER_BOUND('',#1430,.T.);
#974=FACE_OUTER_BOUND('',#1431,.T.);
#975=FACE_OUTER_BOUND('',#1432,.T.);
#976=FACE_OUTER_BOUND('',#1433,.T.);
#977=FACE_OUTER_BOUND('',#1435,.T.);
#978=FACE_OUTER_BOUND('',#1436,.T.);
#979=FACE_OUTER_BOUND('',#1437,.T.);
#980=FACE_OUTER_BOUND('',#1438,.T.);
#981=FACE_OUTER_BOUND('',#1440,.T.);
#982=FACE_OUTER_BOUND('',#1442,.T.);
#983=FACE_OUTER_BOUND('',#1443,.T.);
#984=FACE_OUTER_BOUND('',#1444,.T.);
#985=FACE_OUTER_BOUND('',#1445,.T.);
#986=FACE_OUTER_BOUND('',#1446,.T.);
#987=FACE_OUTER_BOUND('',#1448,.T.);
#988=FACE_OUTER_BOUND('',#1449,.T.);
#989=FACE_OUTER_BOUND('',#1450,.T.);
#990=FACE_OUTER_BOUND('',#1451,.T.);
#991=FACE_OUTER_BOUND('',#1452,.T.);
#992=FACE_OUTER_BOUND('',#1453,.T.);
#993=FACE_OUTER_BOUND('',#1454,.T.);
#994=FACE_OUTER_BOUND('',#1455,.T.);
#995=FACE_OUTER_BOUND('',#1456,.T.);
#996=FACE_OUTER_BOUND('',#1457,.T.);
#997=FACE_OUTER_BOUND('',#1458,.T.);
#998=FACE_OUTER_BOUND('',#1459,.T.);
#999=FACE_OUTER_BOUND('',#1460,.T.);
#1000=FACE_OUTER_BOUND('',#1461,.T.);
#1001=FACE_OUTER_BOUND('',#1462,.T.);
#1002=FACE_OUTER_BOUND('',#1463,.T.);
#1003=FACE_OUTER_BOUND('',#1464,.T.);
#1004=FACE_OUTER_BOUND('',#1466,.T.);
#1005=FACE_OUTER_BOUND('',#1467,.T.);
#1006=FACE_OUTER_BOUND('',#1469,.T.);
#1007=FACE_OUTER_BOUND('',#1470,.T.);
#1008=FACE_OUTER_BOUND('',#1471,.T.);
#1009=FACE_OUTER_BOUND('',#1473,.T.);
#1010=FACE_OUTER_BOUND('',#1474,.T.);
#1011=FACE_OUTER_BOUND('',#1475,.T.);
#1012=FACE_OUTER_BOUND('',#1477,.T.);
#1013=FACE_OUTER_BOUND('',#1478,.T.);
#1014=FACE_OUTER_BOUND('',#1480,.T.);
#1015=FACE_OUTER_BOUND('',#1482,.T.);
#1016=FACE_OUTER_BOUND('',#1483,.T.);
#1017=FACE_OUTER_BOUND('',#1485,.T.);
#1018=FACE_OUTER_BOUND('',#1486,.T.);
#1019=FACE_OUTER_BOUND('',#1488,.T.);
#1020=FACE_OUTER_BOUND('',#1490,.T.);
#1021=FACE_OUTER_BOUND('',#1491,.T.);
#1022=FACE_OUTER_BOUND('',#1492,.T.);
#1023=FACE_OUTER_BOUND('',#1493,.T.);
#1024=FACE_OUTER_BOUND('',#1494,.T.);
#1025=FACE_OUTER_BOUND('',#1495,.T.);
#1026=FACE_OUTER_BOUND('',#1496,.T.);
#1027=FACE_OUTER_BOUND('',#1497,.T.);
#1028=FACE_OUTER_BOUND('',#1499,.T.);
#1029=FACE_OUTER_BOUND('',#1500,.T.);
#1030=FACE_OUTER_BOUND('',#1501,.T.);
#1031=FACE_OUTER_BOUND('',#1502,.T.);
#1032=FACE_OUTER_BOUND('',#1504,.T.);
#1033=FACE_OUTER_BOUND('',#1505,.T.);
#1034=FACE_OUTER_BOUND('',#1506,.T.);
#1035=FACE_OUTER_BOUND('',#1507,.T.);
#1036=FACE_OUTER_BOUND('',#1508,.T.);
#1037=FACE_OUTER_BOUND('',#1509,.T.);
#1038=FACE_OUTER_BOUND('',#1510,.T.);
#1039=FACE_OUTER_BOUND('',#1511,.T.);
#1040=FACE_OUTER_BOUND('',#1512,.T.);
#1041=FACE_OUTER_BOUND('',#1513,.T.);
#1042=FACE_OUTER_BOUND('',#1514,.T.);
#1043=FACE_OUTER_BOUND('',#1515,.T.);
#1044=FACE_OUTER_BOUND('',#1516,.T.);
#1045=FACE_OUTER_BOUND('',#1518,.T.);
#1046=FACE_OUTER_BOUND('',#1519,.T.);
#1047=FACE_OUTER_BOUND('',#1520,.T.);
#1048=FACE_OUTER_BOUND('',#1521,.T.);
#1049=FACE_OUTER_BOUND('',#1522,.T.);
#1050=FACE_OUTER_BOUND('',#1523,.T.);
#1051=FACE_OUTER_BOUND('',#1524,.T.);
#1052=FACE_OUTER_BOUND('',#1527,.T.);
#1053=FACE_OUTER_BOUND('',#1528,.T.);
#1054=FACE_OUTER_BOUND('',#1529,.T.);
#1055=FACE_OUTER_BOUND('',#1530,.T.);
#1056=FACE_OUTER_BOUND('',#1531,.T.);
#1057=FACE_OUTER_BOUND('',#1532,.T.);
#1058=FACE_OUTER_BOUND('',#1533,.T.);
#1059=FACE_OUTER_BOUND('',#1534,.T.);
#1060=FACE_OUTER_BOUND('',#1535,.T.);
#1061=FACE_OUTER_BOUND('',#1536,.T.);
#1062=FACE_OUTER_BOUND('',#1537,.T.);
#1063=FACE_OUTER_BOUND('',#1539,.T.);
#1064=FACE_OUTER_BOUND('',#1540,.T.);
#1065=FACE_OUTER_BOUND('',#1541,.T.);
#1066=FACE_OUTER_BOUND('',#1542,.T.);
#1067=FACE_OUTER_BOUND('',#1543,.T.);
#1068=FACE_OUTER_BOUND('',#1544,.T.);
#1069=FACE_OUTER_BOUND('',#1545,.T.);
#1070=FACE_OUTER_BOUND('',#1546,.T.);
#1071=FACE_OUTER_BOUND('',#1547,.T.);
#1072=FACE_OUTER_BOUND('',#1548,.T.);
#1073=FACE_OUTER_BOUND('',#1549,.T.);
#1074=FACE_OUTER_BOUND('',#1551,.T.);
#1075=FACE_OUTER_BOUND('',#1552,.T.);
#1076=FACE_OUTER_BOUND('',#1553,.T.);
#1077=FACE_OUTER_BOUND('',#1554,.T.);
#1078=FACE_OUTER_BOUND('',#1555,.T.);
#1079=FACE_OUTER_BOUND('',#1556,.T.);
#1080=FACE_OUTER_BOUND('',#1557,.T.);
#1081=FACE_OUTER_BOUND('',#1558,.T.);
#1082=FACE_OUTER_BOUND('',#1559,.T.);
#1083=FACE_OUTER_BOUND('',#1561,.T.);
#1084=FACE_OUTER_BOUND('',#1563,.T.);
#1085=FACE_OUTER_BOUND('',#1564,.T.);
#1086=FACE_OUTER_BOUND('',#1565,.T.);
#1087=FACE_OUTER_BOUND('',#1567,.T.);
#1088=FACE_OUTER_BOUND('',#1569,.T.);
#1089=FACE_OUTER_BOUND('',#1570,.T.);
#1090=FACE_OUTER_BOUND('',#1571,.T.);
#1091=FACE_OUTER_BOUND('',#1572,.T.);
#1092=FACE_OUTER_BOUND('',#1573,.T.);
#1093=FACE_OUTER_BOUND('',#1574,.T.);
#1094=FACE_OUTER_BOUND('',#1575,.T.);
#1095=FACE_OUTER_BOUND('',#1576,.T.);
#1096=FACE_OUTER_BOUND('',#1577,.T.);
#1097=FACE_OUTER_BOUND('',#1578,.T.);
#1098=FACE_OUTER_BOUND('',#1579,.T.);
#1099=FACE_OUTER_BOUND('',#1580,.T.);
#1100=FACE_OUTER_BOUND('',#1581,.T.);
#1101=FACE_OUTER_BOUND('',#1582,.T.);
#1102=FACE_OUTER_BOUND('',#1583,.T.);
#1103=FACE_OUTER_BOUND('',#1584,.T.);
#1104=FACE_OUTER_BOUND('',#1585,.T.);
#1105=FACE_OUTER_BOUND('',#1586,.T.);
#1106=FACE_OUTER_BOUND('',#1587,.T.);
#1107=FACE_OUTER_BOUND('',#1588,.T.);
#1108=FACE_OUTER_BOUND('',#1590,.T.);
#1109=FACE_OUTER_BOUND('',#1591,.T.);
#1110=EDGE_LOOP('',(#3973,#3974,#3975,#3976));
#1111=EDGE_LOOP('',(#3977));
#1112=EDGE_LOOP('',(#3978));
#1113=EDGE_LOOP('',(#3979,#3980,#3981,#3982));
#1114=EDGE_LOOP('',(#3983));
#1115=EDGE_LOOP('',(#3984));
#1116=EDGE_LOOP('',(#3985,#3986,#3987,#3988));
#1117=EDGE_LOOP('',(#3989,#3990,#3991,#3992));
#1118=EDGE_LOOP('',(#3993));
#1119=EDGE_LOOP('',(#3994));
#1120=EDGE_LOOP('',(#3995));
#1121=EDGE_LOOP('',(#3996));
#1122=EDGE_LOOP('',(#3997,#3998,#3999,#4000));
#1123=EDGE_LOOP('',(#4001));
#1124=EDGE_LOOP('',(#4002));
#1125=EDGE_LOOP('',(#4003,#4004,#4005,#4006));
#1126=EDGE_LOOP('',(#4007));
#1127=EDGE_LOOP('',(#4008));
#1128=EDGE_LOOP('',(#4009,#4010,#4011,#4012));
#1129=EDGE_LOOP('',(#4013,#4014,#4015,#4016));
#1130=EDGE_LOOP('',(#4017));
#1131=EDGE_LOOP('',(#4018));
#1132=EDGE_LOOP('',(#4019));
#1133=EDGE_LOOP('',(#4020));
#1134=EDGE_LOOP('',(#4021,#4022,#4023,#4024));
#1135=EDGE_LOOP('',(#4025,#4026,#4027,#4028));
#1136=EDGE_LOOP('',(#4029,#4030,#4031,#4032));
#1137=EDGE_LOOP('',(#4033,#4034,#4035,#4036));
#1138=EDGE_LOOP('',(#4037,#4038,#4039,#4040));
#1139=EDGE_LOOP('',(#4041,#4042,#4043,#4044));
#1140=EDGE_LOOP('',(#4045));
#1141=EDGE_LOOP('',(#4046));
#1142=EDGE_LOOP('',(#4047,#4048,#4049,#4050));
#1143=EDGE_LOOP('',(#4051));
#1144=EDGE_LOOP('',(#4052,#4053,#4054,#4055));
#1145=EDGE_LOOP('',(#4056,#4057,#4058,#4059));
#1146=EDGE_LOOP('',(#4060));
#1147=EDGE_LOOP('',(#4061,#4062,#4063,#4064));
#1148=EDGE_LOOP('',(#4065));
#1149=EDGE_LOOP('',(#4066,#4067,#4068,#4069,#4070,#4071,#4072,#4073));
#1150=EDGE_LOOP('',(#4074,#4075,#4076,#4077));
#1151=EDGE_LOOP('',(#4078,#4079,#4080,#4081));
#1152=EDGE_LOOP('',(#4082,#4083,#4084,#4085));
#1153=EDGE_LOOP('',(#4086,#4087,#4088,#4089));
#1154=EDGE_LOOP('',(#4090,#4091,#4092,#4093));
#1155=EDGE_LOOP('',(#4094));
#1156=EDGE_LOOP('',(#4095,#4096,#4097,#4098,#4099,#4100,#4101,#4102));
#1157=EDGE_LOOP('',(#4103,#4104,#4105,#4106));
#1158=EDGE_LOOP('',(#4107));
#1159=EDGE_LOOP('',(#4108,#4109,#4110,#4111));
#1160=EDGE_LOOP('',(#4112,#4113,#4114,#4115));
#1161=EDGE_LOOP('',(#4116));
#1162=EDGE_LOOP('',(#4117,#4118,#4119,#4120));
#1163=EDGE_LOOP('',(#4121));
#1164=EDGE_LOOP('',(#4122,#4123,#4124,#4125,#4126,#4127,#4128,#4129));
#1165=EDGE_LOOP('',(#4130,#4131,#4132,#4133));
#1166=EDGE_LOOP('',(#4134,#4135,#4136,#4137));
#1167=EDGE_LOOP('',(#4138,#4139,#4140,#4141));
#1168=EDGE_LOOP('',(#4142,#4143,#4144,#4145));
#1169=EDGE_LOOP('',(#4146,#4147,#4148,#4149));
#1170=EDGE_LOOP('',(#4150));
#1171=EDGE_LOOP('',(#4151,#4152,#4153,#4154,#4155,#4156,#4157,#4158));
#1172=EDGE_LOOP('',(#4159,#4160,#4161,#4162));
#1173=EDGE_LOOP('',(#4163,#4164,#4165,#4166));
#1174=EDGE_LOOP('',(#4167,#4168,#4169,#4170));
#1175=EDGE_LOOP('',(#4171,#4172,#4173,#4174));
#1176=EDGE_LOOP('',(#4175));
#1177=EDGE_LOOP('',(#4176));
#1178=EDGE_LOOP('',(#4177));
#1179=EDGE_LOOP('',(#4178));
#1180=EDGE_LOOP('',(#4179));
#1181=EDGE_LOOP('',(#4180,#4181,#4182,#4183));
#1182=EDGE_LOOP('',(#4184,#4185,#4186,#4187));
#1183=EDGE_LOOP('',(#4188));
#1184=EDGE_LOOP('',(#4189));
#1185=EDGE_LOOP('',(#4190));
#1186=EDGE_LOOP('',(#4191));
#1187=EDGE_LOOP('',(#4192));
#1188=EDGE_LOOP('',(#4193,#4194,#4195,#4196));
#1189=EDGE_LOOP('',(#4197,#4198,#4199,#4200));
#1190=EDGE_LOOP('',(#4201,#4202,#4203,#4204));
#1191=EDGE_LOOP('',(#4205,#4206,#4207,#4208));
#1192=EDGE_LOOP('',(#4209,#4210,#4211,#4212));
#1193=EDGE_LOOP('',(#4213,#4214,#4215,#4216));
#1194=EDGE_LOOP('',(#4217,#4218,#4219,#4220));
#1195=EDGE_LOOP('',(#4221,#4222,#4223,#4224));
#1196=EDGE_LOOP('',(#4225,#4226,#4227,#4228));
#1197=EDGE_LOOP('',(#4229,#4230,#4231,#4232,#4233,#4234));
#1198=EDGE_LOOP('',(#4235));
#1199=EDGE_LOOP('',(#4236,#4237,#4238,#4239,#4240,#4241));
#1200=EDGE_LOOP('',(#4242));
#1201=EDGE_LOOP('',(#4243));
#1202=EDGE_LOOP('',(#4244));
#1203=EDGE_LOOP('',(#4245,#4246,#4247,#4248));
#1204=EDGE_LOOP('',(#4249));
#1205=EDGE_LOOP('',(#4250));
#1206=EDGE_LOOP('',(#4251,#4252,#4253,#4254));
#1207=EDGE_LOOP('',(#4255,#4256,#4257,#4258));
#1208=EDGE_LOOP('',(#4259));
#1209=EDGE_LOOP('',(#4260));
#1210=EDGE_LOOP('',(#4261,#4262,#4263,#4264));
#1211=EDGE_LOOP('',(#4265,#4266,#4267,#4268));
#1212=EDGE_LOOP('',(#4269));
#1213=EDGE_LOOP('',(#4270));
#1214=EDGE_LOOP('',(#4271,#4272,#4273,#4274));
#1215=EDGE_LOOP('',(#4275,#4276,#4277,#4278));
#1216=EDGE_LOOP('',(#4279,#4280,#4281,#4282,#4283,#4284));
#1217=EDGE_LOOP('',(#4285));
#1218=EDGE_LOOP('',(#4286,#4287,#4288,#4289));
#1219=EDGE_LOOP('',(#4290,#4291,#4292,#4293));
#1220=EDGE_LOOP('',(#4294,#4295,#4296,#4297));
#1221=EDGE_LOOP('',(#4298,#4299,#4300,#4301));
#1222=EDGE_LOOP('',(#4302,#4303,#4304,#4305));
#1223=EDGE_LOOP('',(#4306,#4307,#4308,#4309));
#1224=EDGE_LOOP('',(#4310,#4311,#4312,#4313,#4314,#4315));
#1225=EDGE_LOOP('',(#4316));
#1226=EDGE_LOOP('',(#4317,#4318,#4319,#4320));
#1227=EDGE_LOOP('',(#4321));
#1228=EDGE_LOOP('',(#4322));
#1229=EDGE_LOOP('',(#4323,#4324,#4325,#4326));
#1230=EDGE_LOOP('',(#4327));
#1231=EDGE_LOOP('',(#4328,#4329,#4330,#4331));
#1232=EDGE_LOOP('',(#4332));
#1233=EDGE_LOOP('',(#4333,#4334,#4335,#4336));
#1234=EDGE_LOOP('',(#4337,#4338,#4339,#4340));
#1235=EDGE_LOOP('',(#4341,#4342,#4343,#4344));
#1236=EDGE_LOOP('',(#4345,#4346,#4347,#4348));
#1237=EDGE_LOOP('',(#4349,#4350,#4351,#4352));
#1238=EDGE_LOOP('',(#4353,#4354,#4355,#4356));
#1239=EDGE_LOOP('',(#4357,#4358,#4359,#4360,#4361,#4362));
#1240=EDGE_LOOP('',(#4363));
#1241=EDGE_LOOP('',(#4364));
#1242=EDGE_LOOP('',(#4365,#4366,#4367,#4368));
#1243=EDGE_LOOP('',(#4369,#4370,#4371,#4372));
#1244=EDGE_LOOP('',(#4373));
#1245=EDGE_LOOP('',(#4374));
#1246=EDGE_LOOP('',(#4375));
#1247=EDGE_LOOP('',(#4376));
#1248=EDGE_LOOP('',(#4377,#4378));
#1249=EDGE_LOOP('',(#4379));
#1250=EDGE_LOOP('',(#4380,#4381,#4382,#4383,#4384,#4385,#4386,#4387,#4388,
#4389));
#1251=EDGE_LOOP('',(#4390));
#1252=EDGE_LOOP('',(#4391));
#1253=EDGE_LOOP('',(#4392));
#1254=EDGE_LOOP('',(#4393));
#1255=EDGE_LOOP('',(#4394,#4395,#4396,#4397));
#1256=EDGE_LOOP('',(#4398,#4399,#4400,#4401));
#1257=EDGE_LOOP('',(#4402));
#1258=EDGE_LOOP('',(#4403));
#1259=EDGE_LOOP('',(#4404));
#1260=EDGE_LOOP('',(#4405));
#1261=EDGE_LOOP('',(#4406));
#1262=EDGE_LOOP('',(#4407,#4408,#4409,#4410));
#1263=EDGE_LOOP('',(#4411,#4412,#4413,#4414));
#1264=EDGE_LOOP('',(#4415,#4416,#4417,#4418));
#1265=EDGE_LOOP('',(#4419));
#1266=EDGE_LOOP('',(#4420,#4421,#4422,#4423));
#1267=EDGE_LOOP('',(#4424));
#1268=EDGE_LOOP('',(#4425,#4426,#4427,#4428));
#1269=EDGE_LOOP('',(#4429,#4430,#4431,#4432));
#1270=EDGE_LOOP('',(#4433,#4434,#4435,#4436));
#1271=EDGE_LOOP('',(#4437,#4438,#4439,#4440));
#1272=EDGE_LOOP('',(#4441,#4442,#4443,#4444));
#1273=EDGE_LOOP('',(#4445,#4446,#4447,#4448));
#1274=EDGE_LOOP('',(#4449,#4450,#4451,#4452,#4453,#4454));
#1275=EDGE_LOOP('',(#4455));
#1276=EDGE_LOOP('',(#4456));
#1277=EDGE_LOOP('',(#4457,#4458,#4459,#4460));
#1278=EDGE_LOOP('',(#4461,#4462,#4463,#4464));
#1279=EDGE_LOOP('',(#4465));
#1280=EDGE_LOOP('',(#4466));
#1281=EDGE_LOOP('',(#4467));
#1282=EDGE_LOOP('',(#4468));
#1283=EDGE_LOOP('',(#4469,#4470));
#1284=EDGE_LOOP('',(#4471));
#1285=EDGE_LOOP('',(#4472,#4473,#4474,#4475));
#1286=EDGE_LOOP('',(#4476));
#1287=EDGE_LOOP('',(#4477));
#1288=EDGE_LOOP('',(#4478));
#1289=EDGE_LOOP('',(#4479));
#1290=EDGE_LOOP('',(#4480));
#1291=EDGE_LOOP('',(#4481,#4482,#4483,#4484));
#1292=EDGE_LOOP('',(#4485,#4486,#4487,#4488,#4489,#4490,#4491,#4492,#4493,
#4494));
#1293=EDGE_LOOP('',(#4495));
#1294=EDGE_LOOP('',(#4496));
#1295=EDGE_LOOP('',(#4497));
#1296=EDGE_LOOP('',(#4498));
#1297=EDGE_LOOP('',(#4499,#4500,#4501,#4502));
#1298=EDGE_LOOP('',(#4503,#4504,#4505,#4506));
#1299=EDGE_LOOP('',(#4507,#4508,#4509,#4510));
#1300=EDGE_LOOP('',(#4511,#4512,#4513,#4514));
#1301=EDGE_LOOP('',(#4515,#4516,#4517,#4518));
#1302=EDGE_LOOP('',(#4519,#4520,#4521,#4522));
#1303=EDGE_LOOP('',(#4523,#4524,#4525,#4526));
#1304=EDGE_LOOP('',(#4527,#4528,#4529,#4530));
#1305=EDGE_LOOP('',(#4531,#4532,#4533,#4534));
#1306=EDGE_LOOP('',(#4535,#4536,#4537,#4538));
#1307=EDGE_LOOP('',(#4539,#4540,#4541,#4542,#4543,#4544,#4545,#4546,#4547,
#4548));
#1308=EDGE_LOOP('',(#4549));
#1309=EDGE_LOOP('',(#4550));
#1310=EDGE_LOOP('',(#4551));
#1311=EDGE_LOOP('',(#4552));
#1312=EDGE_LOOP('',(#4553,#4554,#4555,#4556));
#1313=EDGE_LOOP('',(#4557,#4558,#4559,#4560));
#1314=EDGE_LOOP('',(#4561,#4562,#4563,#4564));
#1315=EDGE_LOOP('',(#4565,#4566,#4567,#4568));
#1316=EDGE_LOOP('',(#4569,#4570,#4571,#4572));
#1317=EDGE_LOOP('',(#4573,#4574,#4575,#4576));
#1318=EDGE_LOOP('',(#4577,#4578,#4579,#4580,#4581,#4582,#4583,#4584,#4585,
#4586));
#1319=EDGE_LOOP('',(#4587));
#1320=EDGE_LOOP('',(#4588));
#1321=EDGE_LOOP('',(#4589));
#1322=EDGE_LOOP('',(#4590));
#1323=EDGE_LOOP('',(#4591));
#1324=EDGE_LOOP('',(#4592));
#1325=EDGE_LOOP('',(#4593,#4594,#4595,#4596));
#1326=EDGE_LOOP('',(#4597));
#1327=EDGE_LOOP('',(#4598));
#1328=EDGE_LOOP('',(#4599,#4600,#4601,#4602));
#1329=EDGE_LOOP('',(#4603,#4604,#4605,#4606));
#1330=EDGE_LOOP('',(#4607));
#1331=EDGE_LOOP('',(#4608));
#1332=EDGE_LOOP('',(#4609,#4610,#4611,#4612));
#1333=EDGE_LOOP('',(#4613,#4614,#4615,#4616));
#1334=EDGE_LOOP('',(#4617));
#1335=EDGE_LOOP('',(#4618));
#1336=EDGE_LOOP('',(#4619,#4620,#4621,#4622));
#1337=EDGE_LOOP('',(#4623,#4624,#4625,#4626));
#1338=EDGE_LOOP('',(#4627));
#1339=EDGE_LOOP('',(#4628));
#1340=EDGE_LOOP('',(#4629));
#1341=EDGE_LOOP('',(#4630));
#1342=EDGE_LOOP('',(#4631,#4632,#4633,#4634));
#1343=EDGE_LOOP('',(#4635));
#1344=EDGE_LOOP('',(#4636,#4637,#4638,#4639));
#1345=EDGE_LOOP('',(#4640));
#1346=EDGE_LOOP('',(#4641,#4642,#4643,#4644));
#1347=EDGE_LOOP('',(#4645,#4646,#4647,#4648));
#1348=EDGE_LOOP('',(#4649,#4650,#4651,#4652));
#1349=EDGE_LOOP('',(#4653,#4654,#4655,#4656));
#1350=EDGE_LOOP('',(#4657,#4658,#4659,#4660));
#1351=EDGE_LOOP('',(#4661,#4662,#4663,#4664));
#1352=EDGE_LOOP('',(#4665,#4666,#4667,#4668));
#1353=EDGE_LOOP('',(#4669,#4670,#4671,#4672));
#1354=EDGE_LOOP('',(#4673,#4674,#4675,#4676));
#1355=EDGE_LOOP('',(#4677,#4678,#4679,#4680));
#1356=EDGE_LOOP('',(#4681));
#1357=EDGE_LOOP('',(#4682));
#1358=EDGE_LOOP('',(#4683));
#1359=EDGE_LOOP('',(#4684));
#1360=EDGE_LOOP('',(#4685));
#1361=EDGE_LOOP('',(#4686));
#1362=EDGE_LOOP('',(#4687));
#1363=EDGE_LOOP('',(#4688,#4689,#4690,#4691));
#1364=EDGE_LOOP('',(#4692));
#1365=EDGE_LOOP('',(#4693));
#1366=EDGE_LOOP('',(#4694));
#1367=EDGE_LOOP('',(#4695));
#1368=EDGE_LOOP('',(#4696));
#1369=EDGE_LOOP('',(#4697));
#1370=EDGE_LOOP('',(#4698));
#1371=EDGE_LOOP('',(#4699,#4700,#4701,#4702));
#1372=EDGE_LOOP('',(#4703,#4704,#4705,#4706));
#1373=EDGE_LOOP('',(#4707));
#1374=EDGE_LOOP('',(#4708));
#1375=EDGE_LOOP('',(#4709));
#1376=EDGE_LOOP('',(#4710));
#1377=EDGE_LOOP('',(#4711,#4712,#4713,#4714));
#1378=EDGE_LOOP('',(#4715,#4716,#4717,#4718));
#1379=EDGE_LOOP('',(#4719,#4720,#4721,#4722));
#1380=EDGE_LOOP('',(#4723,#4724,#4725,#4726));
#1381=EDGE_LOOP('',(#4727,#4728,#4729,#4730));
#1382=EDGE_LOOP('',(#4731,#4732,#4733,#4734));
#1383=EDGE_LOOP('',(#4735,#4736,#4737,#4738,#4739,#4740));
#1384=EDGE_LOOP('',(#4741,#4742,#4743,#4744,#4745,#4746));
#1385=EDGE_LOOP('',(#4747));
#1386=EDGE_LOOP('',(#4748));
#1387=EDGE_LOOP('',(#4749,#4750,#4751,#4752));
#1388=EDGE_LOOP('',(#4753));
#1389=EDGE_LOOP('',(#4754));
#1390=EDGE_LOOP('',(#4755,#4756,#4757,#4758));
#1391=EDGE_LOOP('',(#4759,#4760,#4761,#4762));
#1392=EDGE_LOOP('',(#4763,#4764,#4765,#4766));
#1393=EDGE_LOOP('',(#4767));
#1394=EDGE_LOOP('',(#4768));
#1395=EDGE_LOOP('',(#4769,#4770,#4771,#4772));
#1396=EDGE_LOOP('',(#4773,#4774,#4775,#4776));
#1397=EDGE_LOOP('',(#4777,#4778,#4779,#4780));
#1398=EDGE_LOOP('',(#4781,#4782,#4783,#4784));
#1399=EDGE_LOOP('',(#4785));
#1400=EDGE_LOOP('',(#4786));
#1401=EDGE_LOOP('',(#4787,#4788,#4789,#4790));
#1402=EDGE_LOOP('',(#4791));
#1403=EDGE_LOOP('',(#4792));
#1404=EDGE_LOOP('',(#4793,#4794,#4795,#4796,#4797,#4798,#4799,#4800,#4801));
#1405=EDGE_LOOP('',(#4802,#4803,#4804,#4805,#4806,#4807,#4808,#4809,#4810));
#1406=EDGE_LOOP('',(#4811,#4812,#4813,#4814));
#1407=EDGE_LOOP('',(#4815,#4816,#4817,#4818));
#1408=EDGE_LOOP('',(#4819,#4820,#4821,#4822));
#1409=EDGE_LOOP('',(#4823,#4824,#4825,#4826));
#1410=EDGE_LOOP('',(#4827,#4828,#4829,#4830));
#1411=EDGE_LOOP('',(#4831,#4832,#4833,#4834));
#1412=EDGE_LOOP('',(#4835,#4836,#4837,#4838));
#1413=EDGE_LOOP('',(#4839));
#1414=EDGE_LOOP('',(#4840));
#1415=EDGE_LOOP('',(#4841));
#1416=EDGE_LOOP('',(#4842));
#1417=EDGE_LOOP('',(#4843,#4844,#4845,#4846,#4847,#4848));
#1418=EDGE_LOOP('',(#4849));
#1419=EDGE_LOOP('',(#4850,#4851,#4852,#4853,#4854,#4855));
#1420=EDGE_LOOP('',(#4856));
#1421=EDGE_LOOP('',(#4857,#4858,#4859,#4860));
#1422=EDGE_LOOP('',(#4861,#4862,#4863,#4864));
#1423=EDGE_LOOP('',(#4865,#4866,#4867,#4868));
#1424=EDGE_LOOP('',(#4869,#4870,#4871,#4872));
#1425=EDGE_LOOP('',(#4873,#4874,#4875,#4876));
#1426=EDGE_LOOP('',(#4877,#4878,#4879,#4880));
#1427=EDGE_LOOP('',(#4881,#4882,#4883,#4884));
#1428=EDGE_LOOP('',(#4885));
#1429=EDGE_LOOP('',(#4886));
#1430=EDGE_LOOP('',(#4887,#4888,#4889,#4890));
#1431=EDGE_LOOP('',(#4891,#4892,#4893,#4894));
#1432=EDGE_LOOP('',(#4895,#4896,#4897,#4898));
#1433=EDGE_LOOP('',(#4899));
#1434=EDGE_LOOP('',(#4900));
#1435=EDGE_LOOP('',(#4901,#4902,#4903,#4904));
#1436=EDGE_LOOP('',(#4905,#4906,#4907,#4908));
#1437=EDGE_LOOP('',(#4909,#4910,#4911,#4912));
#1438=EDGE_LOOP('',(#4913));
#1439=EDGE_LOOP('',(#4914));
#1440=EDGE_LOOP('',(#4915));
#1441=EDGE_LOOP('',(#4916));
#1442=EDGE_LOOP('',(#4917));
#1443=EDGE_LOOP('',(#4918,#4919,#4920,#4921));
#1444=EDGE_LOOP('',(#4922,#4923,#4924,#4925));
#1445=EDGE_LOOP('',(#4926,#4927,#4928,#4929));
#1446=EDGE_LOOP('',(#4930));
#1447=EDGE_LOOP('',(#4931));
#1448=EDGE_LOOP('',(#4932,#4933,#4934,#4935));
#1449=EDGE_LOOP('',(#4936,#4937,#4938,#4939));
#1450=EDGE_LOOP('',(#4940,#4941,#4942,#4943));
#1451=EDGE_LOOP('',(#4944));
#1452=EDGE_LOOP('',(#4945,#4946,#4947,#4948));
#1453=EDGE_LOOP('',(#4949,#4950,#4951,#4952));
#1454=EDGE_LOOP('',(#4953,#4954,#4955,#4956));
#1455=EDGE_LOOP('',(#4957,#4958,#4959,#4960));
#1456=EDGE_LOOP('',(#4961,#4962,#4963,#4964));
#1457=EDGE_LOOP('',(#4965,#4966,#4967,#4968));
#1458=EDGE_LOOP('',(#4969,#4970,#4971,#4972,#4973,#4974));
#1459=EDGE_LOOP('',(#4975,#4976,#4977,#4978,#4979,#4980));
#1460=EDGE_LOOP('',(#4981,#4982,#4983,#4984));
#1461=EDGE_LOOP('',(#4985));
#1462=EDGE_LOOP('',(#4986));
#1463=EDGE_LOOP('',(#4987,#4988,#4989,#4990,#4991,#4992));
#1464=EDGE_LOOP('',(#4993,#4994));
#1465=EDGE_LOOP('',(#4995,#4996,#4997,#4998));
#1466=EDGE_LOOP('',(#4999,#5000,#5001,#5002,#5003,#5004));
#1467=EDGE_LOOP('',(#5005));
#1468=EDGE_LOOP('',(#5006));
#1469=EDGE_LOOP('',(#5007,#5008,#5009,#5010));
#1470=EDGE_LOOP('',(#5011,#5012,#5013,#5014));
#1471=EDGE_LOOP('',(#5015));
#1472=EDGE_LOOP('',(#5016));
#1473=EDGE_LOOP('',(#5017,#5018,#5019,#5020));
#1474=EDGE_LOOP('',(#5021,#5022,#5023,#5024,#5025,#5026));
#1475=EDGE_LOOP('',(#5027));
#1476=EDGE_LOOP('',(#5028));
#1477=EDGE_LOOP('',(#5029,#5030,#5031,#5032));
#1478=EDGE_LOOP('',(#5033));
#1479=EDGE_LOOP('',(#5034));
#1480=EDGE_LOOP('',(#5035));
#1481=EDGE_LOOP('',(#5036));
#1482=EDGE_LOOP('',(#5037,#5038,#5039,#5040));
#1483=EDGE_LOOP('',(#5041));
#1484=EDGE_LOOP('',(#5042));
#1485=EDGE_LOOP('',(#5043,#5044,#5045,#5046,#5047,#5048));
#1486=EDGE_LOOP('',(#5049,#5050,#5051,#5052,#5053,#5054));
#1487=EDGE_LOOP('',(#5055));
#1488=EDGE_LOOP('',(#5056,#5057,#5058,#5059,#5060,#5061));
#1489=EDGE_LOOP('',(#5062));
#1490=EDGE_LOOP('',(#5063,#5064,#5065,#5066));
#1491=EDGE_LOOP('',(#5067,#5068,#5069,#5070));
#1492=EDGE_LOOP('',(#5071,#5072,#5073,#5074));
#1493=EDGE_LOOP('',(#5075,#5076,#5077,#5078));
#1494=EDGE_LOOP('',(#5079,#5080,#5081,#5082));
#1495=EDGE_LOOP('',(#5083,#5084,#5085,#5086));
#1496=EDGE_LOOP('',(#5087,#5088,#5089,#5090));
#1497=EDGE_LOOP('',(#5091));
#1498=EDGE_LOOP('',(#5092));
#1499=EDGE_LOOP('',(#5093,#5094,#5095,#5096));
#1500=EDGE_LOOP('',(#5097,#5098,#5099,#5100));
#1501=EDGE_LOOP('',(#5101,#5102,#5103,#5104));
#1502=EDGE_LOOP('',(#5105));
#1503=EDGE_LOOP('',(#5106));
#1504=EDGE_LOOP('',(#5107,#5108,#5109,#5110));
#1505=EDGE_LOOP('',(#5111,#5112,#5113,#5114));
#1506=EDGE_LOOP('',(#5115,#5116,#5117,#5118));
#1507=EDGE_LOOP('',(#5119));
#1508=EDGE_LOOP('',(#5120,#5121,#5122,#5123,#5124,#5125,#5126,#5127,#5128));
#1509=EDGE_LOOP('',(#5129,#5130,#5131,#5132));
#1510=EDGE_LOOP('',(#5133,#5134,#5135,#5136));
#1511=EDGE_LOOP('',(#5137,#5138,#5139,#5140));
#1512=EDGE_LOOP('',(#5141,#5142,#5143,#5144));
#1513=EDGE_LOOP('',(#5145,#5146,#5147,#5148));
#1514=EDGE_LOOP('',(#5149,#5150,#5151,#5152));
#1515=EDGE_LOOP('',(#5153));
#1516=EDGE_LOOP('',(#5154,#5155,#5156,#5157,#5158,#5159));
#1517=EDGE_LOOP('',(#5160));
#1518=EDGE_LOOP('',(#5161,#5162,#5163,#5164));
#1519=EDGE_LOOP('',(#5165,#5166,#5167,#5168,#5169));
#1520=EDGE_LOOP('',(#5170,#5171,#5172,#5173));
#1521=EDGE_LOOP('',(#5174,#5175,#5176,#5177));
#1522=EDGE_LOOP('',(#5178,#5179,#5180,#5181));
#1523=EDGE_LOOP('',(#5182,#5183,#5184,#5185));
#1524=EDGE_LOOP('',(#5186,#5187,#5188,#5189,#5190,#5191,#5192));
#1525=EDGE_LOOP('',(#5193));
#1526=EDGE_LOOP('',(#5194));
#1527=EDGE_LOOP('',(#5195,#5196,#5197,#5198));
#1528=EDGE_LOOP('',(#5199));
#1529=EDGE_LOOP('',(#5200,#5201,#5202));
#1530=EDGE_LOOP('',(#5203,#5204,#5205));
#1531=EDGE_LOOP('',(#5206,#5207,#5208));
#1532=EDGE_LOOP('',(#5209,#5210,#5211));
#1533=EDGE_LOOP('',(#5212,#5213,#5214,#5215,#5216,#5217));
#1534=EDGE_LOOP('',(#5218,#5219,#5220,#5221,#5222,#5223));
#1535=EDGE_LOOP('',(#5224,#5225,#5226,#5227,#5228,#5229));
#1536=EDGE_LOOP('',(#5230,#5231,#5232,#5233,#5234,#5235));
#1537=EDGE_LOOP('',(#5236,#5237,#5238,#5239));
#1538=EDGE_LOOP('',(#5240));
#1539=EDGE_LOOP('',(#5241,#5242));
#1540=EDGE_LOOP('',(#5243,#5244,#5245));
#1541=EDGE_LOOP('',(#5246,#5247));
#1542=EDGE_LOOP('',(#5248,#5249));
#1543=EDGE_LOOP('',(#5250,#5251,#5252,#5253));
#1544=EDGE_LOOP('',(#5254,#5255,#5256,#5257));
#1545=EDGE_LOOP('',(#5258,#5259,#5260,#5261));
#1546=EDGE_LOOP('',(#5262,#5263,#5264,#5265));
#1547=EDGE_LOOP('',(#5266,#5267,#5268,#5269));
#1548=EDGE_LOOP('',(#5270,#5271,#5272,#5273,#5274,#5275,#5276,#5277,#5278,
#5279,#5280,#5281));
#1549=EDGE_LOOP('',(#5282));
#1550=EDGE_LOOP('',(#5283,#5284,#5285,#5286));
#1551=EDGE_LOOP('',(#5287,#5288,#5289,#5290));
#1552=EDGE_LOOP('',(#5291,#5292,#5293,#5294));
#1553=EDGE_LOOP('',(#5295,#5296,#5297,#5298));
#1554=EDGE_LOOP('',(#5299,#5300,#5301,#5302));
#1555=EDGE_LOOP('',(#5303,#5304,#5305,#5306));
#1556=EDGE_LOOP('',(#5307,#5308,#5309,#5310));
#1557=EDGE_LOOP('',(#5311,#5312,#5313,#5314));
#1558=EDGE_LOOP('',(#5315,#5316,#5317,#5318));
#1559=EDGE_LOOP('',(#5319,#5320,#5321,#5322));
#1560=EDGE_LOOP('',(#5323,#5324,#5325,#5326));
#1561=EDGE_LOOP('',(#5327,#5328,#5329,#5330));
#1562=EDGE_LOOP('',(#5331,#5332,#5333,#5334));
#1563=EDGE_LOOP('',(#5335,#5336,#5337,#5338));
#1564=EDGE_LOOP('',(#5339,#5340,#5341,#5342));
#1565=EDGE_LOOP('',(#5343));
#1566=EDGE_LOOP('',(#5344));
#1567=EDGE_LOOP('',(#5345));
#1568=EDGE_LOOP('',(#5346));
#1569=EDGE_LOOP('',(#5347,#5348,#5349,#5350));
#1570=EDGE_LOOP('',(#5351,#5352,#5353,#5354));
#1571=EDGE_LOOP('',(#5355,#5356,#5357,#5358));
#1572=EDGE_LOOP('',(#5359,#5360,#5361,#5362));
#1573=EDGE_LOOP('',(#5363,#5364,#5365,#5366));
#1574=EDGE_LOOP('',(#5367,#5368,#5369,#5370));
#1575=EDGE_LOOP('',(#5371,#5372,#5373,#5374));
#1576=EDGE_LOOP('',(#5375,#5376,#5377,#5378));
#1577=EDGE_LOOP('',(#5379,#5380,#5381,#5382));
#1578=EDGE_LOOP('',(#5383,#5384,#5385,#5386));
#1579=EDGE_LOOP('',(#5387,#5388,#5389,#5390));
#1580=EDGE_LOOP('',(#5391,#5392,#5393,#5394));
#1581=EDGE_LOOP('',(#5395,#5396,#5397,#5398,#5399,#5400));
#1582=EDGE_LOOP('',(#5401,#5402,#5403,#5404,#5405,#5406));
#1583=EDGE_LOOP('',(#5407));
#1584=EDGE_LOOP('',(#5408));
#1585=EDGE_LOOP('',(#5409,#5410,#5411,#5412));
#1586=EDGE_LOOP('',(#5413,#5414,#5415,#5416));
#1587=EDGE_LOOP('',(#5417,#5418,#5419,#5420));
#1588=EDGE_LOOP('',(#5421));
#1589=EDGE_LOOP('',(#5422));
#1590=EDGE_LOOP('',(#5423,#5424,#5425,#5426));
#1591=EDGE_LOOP('',(#5427,#5428,#5429,#5430));
#1592=LINE('',#8773,#2056);
#1593=LINE('',#8782,#2057);
#1594=LINE('',#8788,#2058);
#1595=LINE('',#8793,#2059);
#1596=LINE('',#8802,#2060);
#1597=LINE('',#8811,#2061);
#1598=LINE('',#8817,#2062);
#1599=LINE('',#8822,#2063);
#1600=LINE('',#8831,#2064);
#1601=LINE('',#8837,#2065);
#1602=LINE('',#8843,#2066);
#1603=LINE('',#8849,#2067);
#1604=LINE('',#8855,#2068);
#1605=LINE('',#8861,#2069);
#1606=LINE('',#8868,#2070);
#1607=LINE('',#8875,#2071);
#1608=LINE('',#8880,#2072);
#1609=LINE('',#8882,#2073);
#1610=LINE('',#8884,#2074);
#1611=LINE('',#8885,#2075);
#1612=LINE('',#8889,#2076);
#1613=LINE('',#8891,#2077);
#1614=LINE('',#8893,#2078);
#1615=LINE('',#8894,#2079);
#1616=LINE('',#8897,#2080);
#1617=LINE('',#8899,#2081);
#1618=LINE('',#8901,#2082);
#1619=LINE('',#8903,#2083);
#1620=LINE('',#8904,#2084);
#1621=LINE('',#8910,#2085);
#1622=LINE('',#8911,#2086);
#1623=LINE('',#8915,#2087);
#1624=LINE('',#8916,#2088);
#1625=LINE('',#8917,#2089);
#1626=LINE('',#8919,#2090);
#1627=LINE('',#8922,#2091);
#1628=LINE('',#8923,#2092);
#1629=LINE('',#8925,#2093);
#1630=LINE('',#8930,#2094);
#1631=LINE('',#8937,#2095);
#1632=LINE('',#8942,#2096);
#1633=LINE('',#8944,#2097);
#1634=LINE('',#8946,#2098);
#1635=LINE('',#8947,#2099);
#1636=LINE('',#8951,#2100);
#1637=LINE('',#8953,#2101);
#1638=LINE('',#8955,#2102);
#1639=LINE('',#8956,#2103);
#1640=LINE('',#8959,#2104);
#1641=LINE('',#8961,#2105);
#1642=LINE('',#8963,#2106);
#1643=LINE('',#8965,#2107);
#1644=LINE('',#8966,#2108);
#1645=LINE('',#8972,#2109);
#1646=LINE('',#8973,#2110);
#1647=LINE('',#8977,#2111);
#1648=LINE('',#8978,#2112);
#1649=LINE('',#8979,#2113);
#1650=LINE('',#8981,#2114);
#1651=LINE('',#8984,#2115);
#1652=LINE('',#8985,#2116);
#1653=LINE('',#8987,#2117);
#1654=LINE('',#8991,#2118);
#1655=LINE('',#8993,#2119);
#1656=LINE('',#8995,#2120);
#1657=LINE('',#8996,#2121);
#1658=LINE('',#8999,#2122);
#1659=LINE('',#9001,#2123);
#1660=LINE('',#9002,#2124);
#1661=LINE('',#9005,#2125);
#1662=LINE('',#9007,#2126);
#1663=LINE('',#9008,#2127);
#1664=LINE('',#9010,#2128);
#1665=LINE('',#9011,#2129);
#1666=LINE('',#9019,#2130);
#1667=LINE('',#9024,#2131);
#1668=LINE('',#9026,#2132);
#1669=LINE('',#9028,#2133);
#1670=LINE('',#9029,#2134);
#1671=LINE('',#9032,#2135);
#1672=LINE('',#9034,#2136);
#1673=LINE('',#9035,#2137);
#1674=LINE('',#9038,#2138);
#1675=LINE('',#9040,#2139);
#1676=LINE('',#9041,#2140);
#1677=LINE('',#9044,#2141);
#1678=LINE('',#9046,#2142);
#1679=LINE('',#9047,#2143);
#1680=LINE('',#9050,#2144);
#1681=LINE('',#9052,#2145);
#1682=LINE('',#9053,#2146);
#1683=LINE('',#9055,#2147);
#1684=LINE('',#9056,#2148);
#1685=LINE('',#9068,#2149);
#1686=LINE('',#9075,#2150);
#1687=LINE('',#9079,#2151);
#1688=LINE('',#9086,#2152);
#1689=LINE('',#9090,#2153);
#1690=LINE('',#9097,#2154);
#1691=LINE('',#9101,#2155);
#1692=LINE('',#9105,#2156);
#1693=LINE('',#9107,#2157);
#1694=LINE('',#9109,#2158);
#1695=LINE('',#9111,#2159);
#1696=LINE('',#9113,#2160);
#1697=LINE('',#9114,#2161);
#1698=LINE('',#9119,#2162);
#1699=LINE('',#9121,#2163);
#1700=LINE('',#9122,#2164);
#1701=LINE('',#9125,#2165);
#1702=LINE('',#9126,#2166);
#1703=LINE('',#9129,#2167);
#1704=LINE('',#9130,#2168);
#1705=LINE('',#9133,#2169);
#1706=LINE('',#9134,#2170);
#1707=LINE('',#9137,#2171);
#1708=LINE('',#9138,#2172);
#1709=LINE('',#9140,#2173);
#1710=LINE('',#9144,#2174);
#1711=LINE('',#9152,#2175);
#1712=LINE('',#9159,#2176);
#1713=LINE('',#9166,#2177);
#1714=LINE('',#9172,#2178);
#1715=LINE('',#9178,#2179);
#1716=LINE('',#9184,#2180);
#1717=LINE('',#9189,#2181);
#1718=LINE('',#9193,#2182);
#1719=LINE('',#9197,#2183);
#1720=LINE('',#9200,#2184);
#1721=LINE('',#9203,#2185);
#1722=LINE('',#9205,#2186);
#1723=LINE('',#9207,#2187);
#1724=LINE('',#9209,#2188);
#1725=LINE('',#9210,#2189);
#1726=LINE('',#9215,#2190);
#1727=LINE('',#9221,#2191);
#1728=LINE('',#9231,#2192);
#1729=LINE('',#9233,#2193);
#1730=LINE('',#9234,#2194);
#1731=LINE('',#9237,#2195);
#1732=LINE('',#9238,#2196);
#1733=LINE('',#9241,#2197);
#1734=LINE('',#9242,#2198);
#1735=LINE('',#9244,#2199);
#1736=LINE('',#9251,#2200);
#1737=LINE('',#9258,#2201);
#1738=LINE('',#9265,#2202);
#1739=LINE('',#9271,#2203);
#1740=LINE('',#9277,#2204);
#1741=LINE('',#9283,#2205);
#1742=LINE('',#9288,#2206);
#1743=LINE('',#9292,#2207);
#1744=LINE('',#9296,#2208);
#1745=LINE('',#9299,#2209);
#1746=LINE('',#9302,#2210);
#1747=LINE('',#9304,#2211);
#1748=LINE('',#9306,#2212);
#1749=LINE('',#9308,#2213);
#1750=LINE('',#9309,#2214);
#1751=LINE('',#9314,#2215);
#1752=LINE('',#9320,#2216);
#1753=LINE('',#9331,#2217);
#1754=LINE('',#9332,#2218);
#1755=LINE('',#9333,#2219);
#1756=LINE('',#9336,#2220);
#1757=LINE('',#9337,#2221);
#1758=LINE('',#9340,#2222);
#1759=LINE('',#9341,#2223);
#1760=LINE('',#9343,#2224);
#1761=LINE('',#9350,#2225);
#1762=LINE('',#9356,#2226);
#1763=LINE('',#9362,#2227);
#1764=LINE('',#9368,#2228);
#1765=LINE('',#9373,#2229);
#1766=LINE('',#9375,#2230);
#1767=LINE('',#9377,#2231);
#1768=LINE('',#9378,#2232);
#1769=LINE('',#9382,#2233);
#1770=LINE('',#9384,#2234);
#1771=LINE('',#9386,#2235);
#1772=LINE('',#9387,#2236);
#1773=LINE('',#9390,#2237);
#1774=LINE('',#9392,#2238);
#1775=LINE('',#9393,#2239);
#1776=LINE('',#9396,#2240);
#1777=LINE('',#9398,#2241);
#1778=LINE('',#9399,#2242);
#1779=LINE('',#9403,#2243);
#1780=LINE('',#9405,#2244);
#1781=LINE('',#9407,#2245);
#1782=LINE('',#9409,#2246);
#1783=LINE('',#9410,#2247);
#1784=LINE('',#9413,#2248);
#1785=LINE('',#9414,#2249);
#1786=LINE('',#9417,#2250);
#1787=LINE('',#9418,#2251);
#1788=LINE('',#9423,#2252);
#1789=LINE('',#9424,#2253);
#1790=LINE('',#9427,#2254);
#1791=LINE('',#9428,#2255);
#1792=LINE('',#9430,#2256);
#1793=LINE('',#9441,#2257);
#1794=LINE('',#9447,#2258);
#1795=LINE('',#9451,#2259);
#1796=LINE('',#9464,#2260);
#1797=LINE('',#9472,#2261);
#1798=LINE('',#9477,#2262);
#1799=LINE('',#9486,#2263);
#1800=LINE('',#9493,#2264);
#1801=LINE('',#9500,#2265);
#1802=LINE('',#9506,#2266);
#1803=LINE('',#9512,#2267);
#1804=LINE('',#9518,#2268);
#1805=LINE('',#9524,#2269);
#1806=LINE('',#9529,#2270);
#1807=LINE('',#9531,#2271);
#1808=LINE('',#9533,#2272);
#1809=LINE('',#9534,#2273);
#1810=LINE('',#9537,#2274);
#1811=LINE('',#9539,#2275);
#1812=LINE('',#9540,#2276);
#1813=LINE('',#9543,#2277);
#1814=LINE('',#9545,#2278);
#1815=LINE('',#9546,#2279);
#1816=LINE('',#9548,#2280);
#1817=LINE('',#9549,#2281);
#1818=LINE('',#9560,#2282);
#1819=LINE('',#9566,#2283);
#1820=LINE('',#9574,#2284);
#1821=LINE('',#9576,#2285);
#1822=LINE('',#9578,#2286);
#1823=LINE('',#9579,#2287);
#1824=LINE('',#9582,#2288);
#1825=LINE('',#9584,#2289);
#1826=LINE('',#9585,#2290);
#1827=LINE('',#9588,#2291);
#1828=LINE('',#9590,#2292);
#1829=LINE('',#9591,#2293);
#1830=LINE('',#9594,#2294);
#1831=LINE('',#9596,#2295);
#1832=LINE('',#9597,#2296);
#1833=LINE('',#9600,#2297);
#1834=LINE('',#9602,#2298);
#1835=LINE('',#9603,#2299);
#1836=LINE('',#9605,#2300);
#1837=LINE('',#9606,#2301);
#1838=LINE('',#9616,#2302);
#1839=LINE('',#9625,#2303);
#1840=LINE('',#9629,#2304);
#1841=LINE('',#9633,#2305);
#1842=LINE('',#9640,#2306);
#1843=LINE('',#9642,#2307);
#1844=LINE('',#9648,#2308);
#1845=LINE('',#9652,#2309);
#1846=LINE('',#9659,#2310);
#1847=LINE('',#9674,#2311);
#1848=LINE('',#9695,#2312);
#1849=LINE('',#9720,#2313);
#1850=LINE('',#9721,#2314);
#1851=LINE('',#9723,#2315);
#1852=LINE('',#9725,#2316);
#1853=LINE('',#9730,#2317);
#1854=LINE('',#9733,#2318);
#1855=LINE('',#9735,#2319);
#1856=LINE('',#9743,#2320);
#1857=LINE('',#9745,#2321);
#1858=LINE('',#9747,#2322);
#1859=LINE('',#9749,#2323);
#1860=LINE('',#9751,#2324);
#1861=LINE('',#9752,#2325);
#1862=LINE('',#9758,#2326);
#1863=LINE('',#9760,#2327);
#1864=LINE('',#9762,#2328);
#1865=LINE('',#9764,#2329);
#1866=LINE('',#9766,#2330);
#1867=LINE('',#9767,#2331);
#1868=LINE('',#9771,#2332);
#1869=LINE('',#9772,#2333);
#1870=LINE('',#9774,#2334);
#1871=LINE('',#9776,#2335);
#1872=LINE('',#9778,#2336);
#1873=LINE('',#9780,#2337);
#1874=LINE('',#9784,#2338);
#1875=LINE('',#9792,#2339);
#1876=LINE('',#9796,#2340);
#1877=LINE('',#9800,#2341);
#1878=LINE('',#9805,#2342);
#1879=LINE('',#9811,#2343);
#1880=LINE('',#9817,#2344);
#1881=LINE('',#9828,#2345);
#1882=LINE('',#9832,#2346);
#1883=LINE('',#9836,#2347);
#1884=LINE('',#9843,#2348);
#1885=LINE('',#9847,#2349);
#1886=LINE('',#9851,#2350);
#1887=LINE('',#9856,#2351);
#1888=LINE('',#9858,#2352);
#1889=LINE('',#9860,#2353);
#1890=LINE('',#9861,#2354);
#1891=LINE('',#9864,#2355);
#1892=LINE('',#9866,#2356);
#1893=LINE('',#9867,#2357);
#1894=LINE('',#9870,#2358);
#1895=LINE('',#9872,#2359);
#1896=LINE('',#9873,#2360);
#1897=LINE('',#9876,#2361);
#1898=LINE('',#9878,#2362);
#1899=LINE('',#9879,#2363);
#1900=LINE('',#9882,#2364);
#1901=LINE('',#9884,#2365);
#1902=LINE('',#9885,#2366);
#1903=LINE('',#9887,#2367);
#1904=LINE('',#9888,#2368);
#1905=LINE('',#9896,#2369);
#1906=LINE('',#9908,#2370);
#1907=LINE('',#9920,#2371);
#1908=LINE('',#9928,#2372);
#1909=LINE('',#9933,#2373);
#1910=LINE('',#9948,#2374);
#1911=LINE('',#9956,#2375);
#1912=LINE('',#9966,#2376);
#1913=LINE('',#9969,#2377);
#1914=LINE('',#9974,#2378);
#1915=LINE('',#9976,#2379);
#1916=LINE('',#9978,#2380);
#1917=LINE('',#9980,#2381);
#1918=LINE('',#9982,#2382);
#1919=LINE('',#9983,#2383);
#1920=LINE('',#9989,#2384);
#1921=LINE('',#9991,#2385);
#1922=LINE('',#9993,#2386);
#1923=LINE('',#9995,#2387);
#1924=LINE('',#9997,#2388);
#1925=LINE('',#9998,#2389);
#1926=LINE('',#10002,#2390);
#1927=LINE('',#10003,#2391);
#1928=LINE('',#10005,#2392);
#1929=LINE('',#10007,#2393);
#1930=LINE('',#10009,#2394);
#1931=LINE('',#10011,#2395);
#1932=LINE('',#10015,#2396);
#1933=LINE('',#10023,#2397);
#1934=LINE('',#10027,#2398);
#1935=LINE('',#10031,#2399);
#1936=LINE('',#10036,#2400);
#1937=LINE('',#10042,#2401);
#1938=LINE('',#10047,#2402);
#1939=LINE('',#10053,#2403);
#1940=LINE('',#10079,#2404);
#1941=LINE('',#10081,#2405);
#1942=LINE('',#10082,#2406);
#1943=LINE('',#10085,#2407);
#1944=LINE('',#10086,#2408);
#1945=LINE('',#10089,#2409);
#1946=LINE('',#10090,#2410);
#1947=LINE('',#10093,#2411);
#1948=LINE('',#10094,#2412);
#1949=LINE('',#10097,#2413);
#1950=LINE('',#10098,#2414);
#1951=LINE('',#10100,#2415);
#1952=LINE('',#10157,#2416);
#1953=LINE('',#10159,#2417);
#1954=LINE('',#10160,#2418);
#1955=LINE('',#10165,#2419);
#1956=LINE('',#10167,#2420);
#1957=LINE('',#10173,#2421);
#1958=LINE('',#10174,#2422);
#1959=LINE('',#10177,#2423);
#1960=LINE('',#10183,#2424);
#1961=LINE('',#10193,#2425);
#1962=LINE('',#10201,#2426);
#1963=LINE('',#10202,#2427);
#1964=LINE('',#10208,#2428);
#1965=LINE('',#10209,#2429);
#1966=LINE('',#10215,#2430);
#1967=LINE('',#10216,#2431);
#1968=LINE('',#10222,#2432);
#1969=LINE('',#10223,#2433);
#1970=LINE('',#10225,#2434);
#1971=LINE('',#10227,#2435);
#1972=LINE('',#10229,#2436);
#1973=LINE('',#10230,#2437);
#1974=LINE('',#10232,#2438);
#1975=LINE('',#10234,#2439);
#1976=LINE('',#10235,#2440);
#1977=LINE('',#10237,#2441);
#1978=LINE('',#10239,#2442);
#1979=LINE('',#10240,#2443);
#1980=LINE('',#10242,#2444);
#1981=LINE('',#10243,#2445);
#1982=LINE('',#10258,#2446);
#1983=LINE('',#10260,#2447);
#1984=LINE('',#10262,#2448);
#1985=LINE('',#10263,#2449);
#1986=LINE('',#10266,#2450);
#1987=LINE('',#10268,#2451);
#1988=LINE('',#10269,#2452);
#1989=LINE('',#10272,#2453);
#1990=LINE('',#10274,#2454);
#1991=LINE('',#10275,#2455);
#1992=LINE('',#10277,#2456);
#1993=LINE('',#10278,#2457);
#1994=LINE('',#10282,#2458);
#1995=LINE('',#10289,#2459);
#1996=LINE('',#10291,#2460);
#1997=LINE('',#10293,#2461);
#1998=LINE('',#10294,#2462);
#1999=LINE('',#10297,#2463);
#2000=LINE('',#10299,#2464);
#2001=LINE('',#10300,#2465);
#2002=LINE('',#10303,#2466);
#2003=LINE('',#10305,#2467);
#2004=LINE('',#10306,#2468);
#2005=LINE('',#10308,#2469);
#2006=LINE('',#10309,#2470);
#2007=LINE('',#10313,#2471);
#2008=LINE('',#10315,#2472);
#2009=LINE('',#10317,#2473);
#2010=LINE('',#10318,#2474);
#2011=LINE('',#10321,#2475);
#2012=LINE('',#10323,#2476);
#2013=LINE('',#10324,#2477);
#2014=LINE('',#10327,#2478);
#2015=LINE('',#10329,#2479);
#2016=LINE('',#10330,#2480);
#2017=LINE('',#10332,#2481);
#2018=LINE('',#10333,#2482);
#2019=LINE('',#10341,#2483);
#2020=LINE('',#10347,#2484);
#2021=LINE('',#10355,#2485);
#2022=LINE('',#10357,#2486);
#2023=LINE('',#10359,#2487);
#2024=LINE('',#10360,#2488);
#2025=LINE('',#10363,#2489);
#2026=LINE('',#10365,#2490);
#2027=LINE('',#10366,#2491);
#2028=LINE('',#10369,#2492);
#2029=LINE('',#10371,#2493);
#2030=LINE('',#10372,#2494);
#2031=LINE('',#10374,#2495);
#2032=LINE('',#10375,#2496);
#2033=LINE('',#10382,#2497);
#2034=LINE('',#10384,#2498);
#2035=LINE('',#10386,#2499);
#2036=LINE('',#10387,#2500);
#2037=LINE('',#10390,#2501);
#2038=LINE('',#10392,#2502);
#2039=LINE('',#10393,#2503);
#2040=LINE('',#10396,#2504);
#2041=LINE('',#10398,#2505);
#2042=LINE('',#10399,#2506);
#2043=LINE('',#10402,#2507);
#2044=LINE('',#10404,#2508);
#2045=LINE('',#10405,#2509);
#2046=LINE('',#10408,#2510);
#2047=LINE('',#10410,#2511);
#2048=LINE('',#10411,#2512);
#2049=LINE('',#10413,#2513);
#2050=LINE('',#10414,#2514);
#2051=LINE('',#10426,#2515);
#2052=LINE('',#10430,#2516);
#2053=LINE('',#10434,#2517);
#2054=LINE('',#10441,#2518);
#2055=LINE('',#10443,#2519);
#2056=VECTOR('',#6934,0.685);
#2057=VECTOR('',#6945,1.065);
#2058=VECTOR('',#6954,0.46);
#2059=VECTOR('',#6959,1.5);
#2060=VECTOR('',#6972,0.685);
#2061=VECTOR('',#6983,1.065);
#2062=VECTOR('',#6992,0.46);
#2063=VECTOR('',#6997,1.5);
#2064=VECTOR('',#7010,0.33);
#2065=VECTOR('',#7017,0.33);
#2066=VECTOR('',#7024,0.33);
#2067=VECTOR('',#7031,0.33);
#2068=VECTOR('',#7038,0.7);
#2069=VECTOR('',#7045,1.1);
#2070=VECTOR('',#7054,0.25);
#2071=VECTOR('',#7063,0.33);
#2072=VECTOR('',#7068,1.);
#2073=VECTOR('',#7069,1.);
#2074=VECTOR('',#7070,1.);
#2075=VECTOR('',#7071,1.);
#2076=VECTOR('',#7074,1.);
#2077=VECTOR('',#7075,1.);
#2078=VECTOR('',#7076,1.);
#2079=VECTOR('',#7077,1.);
#2080=VECTOR('',#7080,1.);
#2081=VECTOR('',#7081,1.);
#2082=VECTOR('',#7082,1.);
#2083=VECTOR('',#7083,1.);
#2084=VECTOR('',#7084,1.);
#2085=VECTOR('',#7093,1.);
#2086=VECTOR('',#7094,1.);
#2087=VECTOR('',#7097,1.);
#2088=VECTOR('',#7098,1.);
#2089=VECTOR('',#7099,1.);
#2090=VECTOR('',#7102,1.);
#2091=VECTOR('',#7105,1.);
#2092=VECTOR('',#7106,1.);
#2093=VECTOR('',#7109,1.);
#2094=VECTOR('',#7114,0.25);
#2095=VECTOR('',#7123,0.33);
#2096=VECTOR('',#7128,1.);
#2097=VECTOR('',#7129,1.);
#2098=VECTOR('',#7130,1.);
#2099=VECTOR('',#7131,1.);
#2100=VECTOR('',#7134,1.);
#2101=VECTOR('',#7135,1.);
#2102=VECTOR('',#7136,1.);
#2103=VECTOR('',#7137,1.);
#2104=VECTOR('',#7140,1.);
#2105=VECTOR('',#7141,1.);
#2106=VECTOR('',#7142,1.);
#2107=VECTOR('',#7143,1.);
#2108=VECTOR('',#7144,1.);
#2109=VECTOR('',#7153,1.);
#2110=VECTOR('',#7154,1.);
#2111=VECTOR('',#7157,1.);
#2112=VECTOR('',#7158,1.);
#2113=VECTOR('',#7159,1.);
#2114=VECTOR('',#7162,1.);
#2115=VECTOR('',#7165,1.);
#2116=VECTOR('',#7166,1.);
#2117=VECTOR('',#7169,1.);
#2118=VECTOR('',#7172,1.);
#2119=VECTOR('',#7173,1.);
#2120=VECTOR('',#7174,1.);
#2121=VECTOR('',#7175,1.);
#2122=VECTOR('',#7178,1.);
#2123=VECTOR('',#7179,1.);
#2124=VECTOR('',#7180,1.);
#2125=VECTOR('',#7183,1.);
#2126=VECTOR('',#7184,1.);
#2127=VECTOR('',#7185,1.);
#2128=VECTOR('',#7188,1.);
#2129=VECTOR('',#7189,1.);
#2130=VECTOR('',#7200,0.57);
#2131=VECTOR('',#7205,1.);
#2132=VECTOR('',#7206,1.);
#2133=VECTOR('',#7207,1.);
#2134=VECTOR('',#7208,1.);
#2135=VECTOR('',#7211,1.);
#2136=VECTOR('',#7212,1.);
#2137=VECTOR('',#7213,1.);
#2138=VECTOR('',#7216,1.);
#2139=VECTOR('',#7217,1.);
#2140=VECTOR('',#7218,1.);
#2141=VECTOR('',#7221,1.);
#2142=VECTOR('',#7222,1.);
#2143=VECTOR('',#7223,1.);
#2144=VECTOR('',#7226,1.);
#2145=VECTOR('',#7227,1.);
#2146=VECTOR('',#7228,1.);
#2147=VECTOR('',#7231,1.);
#2148=VECTOR('',#7232,1.);
#2149=VECTOR('',#7249,0.205);
#2150=VECTOR('',#7258,0.19);
#2151=VECTOR('',#7263,0.205);
#2152=VECTOR('',#7272,0.19);
#2153=VECTOR('',#7277,0.205);
#2154=VECTOR('',#7286,0.19);
#2155=VECTOR('',#7291,0.125);
#2156=VECTOR('',#7294,1.);
#2157=VECTOR('',#7295,1.);
#2158=VECTOR('',#7296,1.);
#2159=VECTOR('',#7297,1.);
#2160=VECTOR('',#7298,1.);
#2161=VECTOR('',#7299,1.);
#2162=VECTOR('',#7304,1.);
#2163=VECTOR('',#7305,1.);
#2164=VECTOR('',#7306,1.);
#2165=VECTOR('',#7309,1.);
#2166=VECTOR('',#7310,1.);
#2167=VECTOR('',#7313,1.);
#2168=VECTOR('',#7314,1.);
#2169=VECTOR('',#7317,1.);
#2170=VECTOR('',#7318,1.);
#2171=VECTOR('',#7321,1.);
#2172=VECTOR('',#7322,1.);
#2173=VECTOR('',#7325,1.);
#2174=VECTOR('',#7330,0.685);
#2175=VECTOR('',#7341,0.165);
#2176=VECTOR('',#7350,0.165);
#2177=VECTOR('',#7359,0.275);
#2178=VECTOR('',#7366,0.275);
#2179=VECTOR('',#7373,0.275);
#2180=VECTOR('',#7380,0.275);
#2181=VECTOR('',#7385,1.);
#2182=VECTOR('',#7388,1.);
#2183=VECTOR('',#7393,1.);
#2184=VECTOR('',#7396,1.);
#2185=VECTOR('',#7399,1.);
#2186=VECTOR('',#7400,1.);
#2187=VECTOR('',#7401,1.);
#2188=VECTOR('',#7402,1.);
#2189=VECTOR('',#7403,1.);
#2190=VECTOR('',#7408,0.93);
#2191=VECTOR('',#7415,1.3);
#2192=VECTOR('',#7430,1.);
#2193=VECTOR('',#7431,1.);
#2194=VECTOR('',#7432,1.);
#2195=VECTOR('',#7435,1.);
#2196=VECTOR('',#7436,1.);
#2197=VECTOR('',#7439,1.);
#2198=VECTOR('',#7440,1.);
#2199=VECTOR('',#7443,1.);
#2200=VECTOR('',#7452,0.165);
#2201=VECTOR('',#7461,0.165);
#2202=VECTOR('',#7470,0.275);
#2203=VECTOR('',#7477,0.275);
#2204=VECTOR('',#7484,0.275);
#2205=VECTOR('',#7491,0.275);
#2206=VECTOR('',#7496,1.);
#2207=VECTOR('',#7499,1.);
#2208=VECTOR('',#7504,1.);
#2209=VECTOR('',#7507,1.);
#2210=VECTOR('',#7510,1.);
#2211=VECTOR('',#7511,1.);
#2212=VECTOR('',#7512,1.);
#2213=VECTOR('',#7513,1.);
#2214=VECTOR('',#7514,1.);
#2215=VECTOR('',#7519,0.93);
#2216=VECTOR('',#7526,1.3);
#2217=VECTOR('',#7541,1.);
#2218=VECTOR('',#7542,1.);
#2219=VECTOR('',#7543,1.);
#2220=VECTOR('',#7546,1.);
#2221=VECTOR('',#7547,1.);
#2222=VECTOR('',#7550,1.);
#2223=VECTOR('',#7551,1.);
#2224=VECTOR('',#7554,1.);
#2225=VECTOR('',#7563,0.275);
#2226=VECTOR('',#7570,0.275);
#2227=VECTOR('',#7577,0.275);
#2228=VECTOR('',#7584,0.275);
#2229=VECTOR('',#7589,1.);
#2230=VECTOR('',#7590,1.);
#2231=VECTOR('',#7591,1.);
#2232=VECTOR('',#7592,1.);
#2233=VECTOR('',#7595,1.);
#2234=VECTOR('',#7596,1.);
#2235=VECTOR('',#7597,1.);
#2236=VECTOR('',#7598,1.);
#2237=VECTOR('',#7601,1.);
#2238=VECTOR('',#7602,1.);
#2239=VECTOR('',#7603,1.);
#2240=VECTOR('',#7606,1.);
#2241=VECTOR('',#7607,1.);
#2242=VECTOR('',#7608,1.);
#2243=VECTOR('',#7613,1.);
#2244=VECTOR('',#7614,1.);
#2245=VECTOR('',#7615,1.);
#2246=VECTOR('',#7616,1.);
#2247=VECTOR('',#7617,1.);
#2248=VECTOR('',#7620,1.);
#2249=VECTOR('',#7621,1.);
#2250=VECTOR('',#7624,1.);
#2251=VECTOR('',#7625,1.);
#2252=VECTOR('',#7632,1.);
#2253=VECTOR('',#7633,1.);
#2254=VECTOR('',#7636,1.);
#2255=VECTOR('',#7637,1.);
#2256=VECTOR('',#7640,1.);
#2257=VECTOR('',#7655,1.2);
#2258=VECTOR('',#7662,0.405);
#2259=VECTOR('',#7667,0.7);
#2260=VECTOR('',#7686,0.61);
#2261=VECTOR('',#7697,0.405);
#2262=VECTOR('',#7702,1.);
#2263=VECTOR('',#7715,0.3);
#2264=VECTOR('',#7724,0.3);
#2265=VECTOR('',#7733,0.225);
#2266=VECTOR('',#7740,0.225);
#2267=VECTOR('',#7747,0.225);
#2268=VECTOR('',#7754,0.225);
#2269=VECTOR('',#7761,1.01);
#2270=VECTOR('',#7766,1.);
#2271=VECTOR('',#7767,1.);
#2272=VECTOR('',#7768,1.);
#2273=VECTOR('',#7769,1.);
#2274=VECTOR('',#7772,1.);
#2275=VECTOR('',#7773,1.);
#2276=VECTOR('',#7774,1.);
#2277=VECTOR('',#7777,1.);
#2278=VECTOR('',#7778,1.);
#2279=VECTOR('',#7779,1.);
#2280=VECTOR('',#7782,1.);
#2281=VECTOR('',#7783,1.);
#2282=VECTOR('',#7798,0.75);
#2283=VECTOR('',#7805,1.3);
#2284=VECTOR('',#7816,1.);
#2285=VECTOR('',#7817,1.);
#2286=VECTOR('',#7818,1.);
#2287=VECTOR('',#7819,1.);
#2288=VECTOR('',#7822,1.);
#2289=VECTOR('',#7823,1.);
#2290=VECTOR('',#7824,1.);
#2291=VECTOR('',#7827,1.);
#2292=VECTOR('',#7828,1.);
#2293=VECTOR('',#7829,1.);
#2294=VECTOR('',#7832,1.);
#2295=VECTOR('',#7833,1.);
#2296=VECTOR('',#7834,1.);
#2297=VECTOR('',#7837,1.);
#2298=VECTOR('',#7838,1.);
#2299=VECTOR('',#7839,1.);
#2300=VECTOR('',#7842,1.);
#2301=VECTOR('',#7843,1.);
#2302=VECTOR('',#7856,0.25);
#2303=VECTOR('',#7869,0.4);
#2304=VECTOR('',#7874,0.425);
#2305=VECTOR('',#7879,0.41);
#2306=VECTOR('',#7888,0.26);
#2307=VECTOR('',#7891,0.25);
#2308=VECTOR('',#7898,0.275);
#2309=VECTOR('',#7903,0.265);
#2310=VECTOR('',#7912,0.5);
#2311=VECTOR('',#7921,0.47094010767585);
#2312=VECTOR('',#7928,0.47094010767585);
#2313=VECTOR('',#7931,1.);
#2314=VECTOR('',#7932,1.);
#2315=VECTOR('',#7935,1.);
#2316=VECTOR('',#7938,1.);
#2317=VECTOR('',#7943,0.25);
#2318=VECTOR('',#7948,1.);
#2319=VECTOR('',#7951,1.);
#2320=VECTOR('',#7962,1.);
#2321=VECTOR('',#7963,1.);
#2322=VECTOR('',#7964,1.);
#2323=VECTOR('',#7965,1.);
#2324=VECTOR('',#7966,1.);
#2325=VECTOR('',#7967,1.);
#2326=VECTOR('',#7972,1.);
#2327=VECTOR('',#7973,1.);
#2328=VECTOR('',#7974,1.);
#2329=VECTOR('',#7975,1.);
#2330=VECTOR('',#7976,1.);
#2331=VECTOR('',#7977,1.);
#2332=VECTOR('',#7982,1.);
#2333=VECTOR('',#7983,1.);
#2334=VECTOR('',#7986,1.);
#2335=VECTOR('',#7989,1.);
#2336=VECTOR('',#7992,1.);
#2337=VECTOR('',#7995,1.);
#2338=VECTOR('',#8000,1.065);
#2339=VECTOR('',#8011,1.025);
#2340=VECTOR('',#8016,1.065);
#2341=VECTOR('',#8021,1.025);
#2342=VECTOR('',#8028,0.79);
#2343=VECTOR('',#8035,0.225);
#2344=VECTOR('',#8042,0.4);
#2345=VECTOR('',#8059,0.325);
#2346=VECTOR('',#8064,0.35);
#2347=VECTOR('',#8069,0.335);
#2348=VECTOR('',#8078,0.21);
#2349=VECTOR('',#8083,0.2);
#2350=VECTOR('',#8088,0.18);
#2351=VECTOR('',#8093,1.);
#2352=VECTOR('',#8094,1.);
#2353=VECTOR('',#8095,1.);
#2354=VECTOR('',#8096,1.);
#2355=VECTOR('',#8099,1.);
#2356=VECTOR('',#8100,1.);
#2357=VECTOR('',#8101,1.);
#2358=VECTOR('',#8104,1.);
#2359=VECTOR('',#8105,1.);
#2360=VECTOR('',#8106,1.);
#2361=VECTOR('',#8109,1.);
#2362=VECTOR('',#8110,1.);
#2363=VECTOR('',#8111,1.);
#2364=VECTOR('',#8114,1.);
#2365=VECTOR('',#8115,1.);
#2366=VECTOR('',#8116,1.);
#2367=VECTOR('',#8119,1.);
#2368=VECTOR('',#8120,1.);
#2369=VECTOR('',#8131,0.3);
#2370=VECTOR('',#8146,0.46);
#2371=VECTOR('',#8161,0.46);
#2372=VECTOR('',#8172,0.57);
#2373=VECTOR('',#8177,0.57);
#2374=VECTOR('',#8196,0.825);
#2375=VECTOR('',#8207,1.);
#2376=VECTOR('',#8220,1.);
#2377=VECTOR('',#8225,0.825);
#2378=VECTOR('',#8230,1.);
#2379=VECTOR('',#8231,1.);
#2380=VECTOR('',#8232,1.);
#2381=VECTOR('',#8233,1.);
#2382=VECTOR('',#8234,1.);
#2383=VECTOR('',#8235,1.);
#2384=VECTOR('',#8240,1.);
#2385=VECTOR('',#8241,1.);
#2386=VECTOR('',#8242,1.);
#2387=VECTOR('',#8243,1.);
#2388=VECTOR('',#8244,1.);
#2389=VECTOR('',#8245,1.);
#2390=VECTOR('',#8250,1.);
#2391=VECTOR('',#8251,1.);
#2392=VECTOR('',#8254,1.);
#2393=VECTOR('',#8257,1.);
#2394=VECTOR('',#8260,1.);
#2395=VECTOR('',#8263,1.);
#2396=VECTOR('',#8268,0.685);
#2397=VECTOR('',#8279,0.645);
#2398=VECTOR('',#8284,0.685);
#2399=VECTOR('',#8289,0.645);
#2400=VECTOR('',#8296,0.46);
#2401=VECTOR('',#8303,0.3);
#2402=VECTOR('',#8310,0.27);
#2403=VECTOR('',#8317,0.576175134594813);
#2404=VECTOR('',#8320,1.);
#2405=VECTOR('',#8321,1.);
#2406=VECTOR('',#8322,1.);
#2407=VECTOR('',#8325,1.);
#2408=VECTOR('',#8326,1.);
#2409=VECTOR('',#8329,1.);
#2410=VECTOR('',#8330,1.);
#2411=VECTOR('',#8333,1.);
#2412=VECTOR('',#8334,1.);
#2413=VECTOR('',#8337,1.);
#2414=VECTOR('',#8338,1.);
#2415=VECTOR('',#8341,1.);
#2416=VECTOR('',#8448,1.);
#2417=VECTOR('',#8449,1.);
#2418=VECTOR('',#8450,1.);
#2419=VECTOR('',#8455,1.);
#2420=VECTOR('',#8456,1.);
#2421=VECTOR('',#8463,1.);
#2422=VECTOR('',#8464,1.);
#2423=VECTOR('',#8469,1.);
#2424=VECTOR('',#8476,0.75);
#2425=VECTOR('',#8489,0.165);
#2426=VECTOR('',#8498,1.);
#2427=VECTOR('',#8499,1.);
#2428=VECTOR('',#8504,1.);
#2429=VECTOR('',#8505,1.);
#2430=VECTOR('',#8510,1.);
#2431=VECTOR('',#8511,1.);
#2432=VECTOR('',#8516,1.);
#2433=VECTOR('',#8517,1.);
#2434=VECTOR('',#8520,1.);
#2435=VECTOR('',#8521,1.);
#2436=VECTOR('',#8522,1.);
#2437=VECTOR('',#8523,1.);
#2438=VECTOR('',#8526,1.);
#2439=VECTOR('',#8527,1.);
#2440=VECTOR('',#8528,1.);
#2441=VECTOR('',#8531,1.);
#2442=VECTOR('',#8532,1.);
#2443=VECTOR('',#8533,1.);
#2444=VECTOR('',#8536,1.);
#2445=VECTOR('',#8537,1.);
#2446=VECTOR('',#8560,1.);
#2447=VECTOR('',#8561,1.);
#2448=VECTOR('',#8562,1.);
#2449=VECTOR('',#8563,1.);
#2450=VECTOR('',#8566,1.);
#2451=VECTOR('',#8567,1.);
#2452=VECTOR('',#8568,1.);
#2453=VECTOR('',#8571,1.);
#2454=VECTOR('',#8572,1.);
#2455=VECTOR('',#8573,1.);
#2456=VECTOR('',#8576,1.);
#2457=VECTOR('',#8577,1.);
#2458=VECTOR('',#8582,0.4);
#2459=VECTOR('',#8591,1.);
#2460=VECTOR('',#8592,1.);
#2461=VECTOR('',#8593,1.);
#2462=VECTOR('',#8594,1.);
#2463=VECTOR('',#8597,1.);
#2464=VECTOR('',#8598,1.);
#2465=VECTOR('',#8599,1.);
#2466=VECTOR('',#8602,1.);
#2467=VECTOR('',#8603,1.);
#2468=VECTOR('',#8604,1.);
#2469=VECTOR('',#8607,1.);
#2470=VECTOR('',#8608,1.);
#2471=VECTOR('',#8611,1.);
#2472=VECTOR('',#8612,1.);
#2473=VECTOR('',#8613,1.);
#2474=VECTOR('',#8614,1.);
#2475=VECTOR('',#8617,1.);
#2476=VECTOR('',#8618,1.);
#2477=VECTOR('',#8619,1.);
#2478=VECTOR('',#8622,1.);
#2479=VECTOR('',#8623,1.);
#2480=VECTOR('',#8624,1.);
#2481=VECTOR('',#8627,1.);
#2482=VECTOR('',#8628,1.);
#2483=VECTOR('',#8639,0.225);
#2484=VECTOR('',#8646,0.6);
#2485=VECTOR('',#8657,1.);
#2486=VECTOR('',#8658,1.);
#2487=VECTOR('',#8659,1.);
#2488=VECTOR('',#8660,1.);
#2489=VECTOR('',#8663,1.);
#2490=VECTOR('',#8664,1.);
#2491=VECTOR('',#8665,1.);
#2492=VECTOR('',#8668,1.);
#2493=VECTOR('',#8669,1.);
#2494=VECTOR('',#8670,1.);
#2495=VECTOR('',#8673,1.);
#2496=VECTOR('',#8674,1.);
#2497=VECTOR('',#8683,1.);
#2498=VECTOR('',#8684,1.);
#2499=VECTOR('',#8685,1.);
#2500=VECTOR('',#8686,1.);
#2501=VECTOR('',#8689,1.);
#2502=VECTOR('',#8690,1.);
#2503=VECTOR('',#8691,1.);
#2504=VECTOR('',#8694,1.);
#2505=VECTOR('',#8695,1.);
#2506=VECTOR('',#8696,1.);
#2507=VECTOR('',#8699,1.);
#2508=VECTOR('',#8700,1.);
#2509=VECTOR('',#8701,1.);
#2510=VECTOR('',#8704,1.);
#2511=VECTOR('',#8705,1.);
#2512=VECTOR('',#8706,1.);
#2513=VECTOR('',#8709,1.);
#2514=VECTOR('',#8710,1.);
#2515=VECTOR('',#8727,0.325);
#2516=VECTOR('',#8732,0.35);
#2517=VECTOR('',#8737,0.335);
#2518=VECTOR('',#8746,0.21);
#2519=VECTOR('',#8749,0.2);
#2520=CIRCLE('',#6239,0.685);
#2521=CIRCLE('',#6240,0.685);
#2522=CIRCLE('',#6242,0.46);
#2523=CIRCLE('',#6244,1.065);
#2524=CIRCLE('',#6245,1.065);
#2525=CIRCLE('',#6247,0.46);
#2526=CIRCLE('',#6250,1.5);
#2527=CIRCLE('',#6251,1.5);
#2528=CIRCLE('',#6256,0.685);
#2529=CIRCLE('',#6257,0.685);
#2530=CIRCLE('',#6259,0.46);
#2531=CIRCLE('',#6261,1.065);
#2532=CIRCLE('',#6262,1.065);
#2533=CIRCLE('',#6264,0.46);
#2534=CIRCLE('',#6267,1.5);
#2535=CIRCLE('',#6268,1.5);
#2536=CIRCLE('',#6273,0.33);
#2537=CIRCLE('',#6274,0.33);
#2538=CIRCLE('',#6276,0.33);
#2539=CIRCLE('',#6277,0.33);
#2540=CIRCLE('',#6279,0.33);
#2541=CIRCLE('',#6280,0.33);
#2542=CIRCLE('',#6282,0.33);
#2543=CIRCLE('',#6283,0.33);
#2544=CIRCLE('',#6285,0.7);
#2545=CIRCLE('',#6286,0.7);
#2546=CIRCLE('',#6288,1.1);
#2547=CIRCLE('',#6289,1.1);
#2548=CIRCLE('',#6292,0.25);
#2549=CIRCLE('',#6293,0.25);
#2550=CIRCLE('',#6296,0.33);
#2551=CIRCLE('',#6297,0.33);
#2552=CIRCLE('',#6301,1.51);
#2553=CIRCLE('',#6303,1.51);
#2554=CIRCLE('',#6310,0.25);
#2555=CIRCLE('',#6311,0.25);
#2556=CIRCLE('',#6314,0.33);
#2557=CIRCLE('',#6315,0.33);
#2558=CIRCLE('',#6319,1.51);
#2559=CIRCLE('',#6321,1.51);
#2560=CIRCLE('',#6335,0.57);
#2561=CIRCLE('',#6336,0.57);
#2562=CIRCLE('',#6347,0.19);
#2563=CIRCLE('',#6348,0.125);
#2564=CIRCLE('',#6350,0.22);
#2565=CIRCLE('',#6352,0.19);
#2566=CIRCLE('',#6354,0.19);
#2567=CIRCLE('',#6356,0.22);
#2568=CIRCLE('',#6358,0.19);
#2569=CIRCLE('',#6360,0.19);
#2570=CIRCLE('',#6362,0.22);
#2571=CIRCLE('',#6364,0.19);
#2572=CIRCLE('',#6366,0.19);
#2573=CIRCLE('',#6368,0.125);
#2574=CIRCLE('',#6370,0.685);
#2575=CIRCLE('',#6379,0.685);
#2576=CIRCLE('',#6383,0.165);
#2577=CIRCLE('',#6384,0.165);
#2578=CIRCLE('',#6387,0.165);
#2579=CIRCLE('',#6388,0.165);
#2580=CIRCLE('',#6391,0.275);
#2581=CIRCLE('',#6392,0.275);
#2582=CIRCLE('',#6394,0.275);
#2583=CIRCLE('',#6395,0.275);
#2584=CIRCLE('',#6397,0.275);
#2585=CIRCLE('',#6398,0.275);
#2586=CIRCLE('',#6400,0.275);
#2587=CIRCLE('',#6401,0.275);
#2588=CIRCLE('',#6403,0.7);
#2589=CIRCLE('',#6404,0.7);
#2590=CIRCLE('',#6406,0.556776436283003);
#2591=CIRCLE('',#6409,0.93);
#2592=CIRCLE('',#6410,0.93);
#2593=CIRCLE('',#6412,1.3);
#2594=CIRCLE('',#6413,1.3);
#2595=CIRCLE('',#6415,1.24899959967968);
#2596=CIRCLE('',#6418,1.59980467557762);
#2597=CIRCLE('',#6426,0.165);
#2598=CIRCLE('',#6427,0.165);
#2599=CIRCLE('',#6430,0.165);
#2600=CIRCLE('',#6431,0.165);
#2601=CIRCLE('',#6434,0.275);
#2602=CIRCLE('',#6435,0.275);
#2603=CIRCLE('',#6437,0.275);
#2604=CIRCLE('',#6438,0.275);
#2605=CIRCLE('',#6440,0.275);
#2606=CIRCLE('',#6441,0.275);
#2607=CIRCLE('',#6443,0.275);
#2608=CIRCLE('',#6444,0.275);
#2609=CIRCLE('',#6446,0.7);
#2610=CIRCLE('',#6447,0.7);
#2611=CIRCLE('',#6449,0.556776436283003);
#2612=CIRCLE('',#6452,0.93);
#2613=CIRCLE('',#6453,0.93);
#2614=CIRCLE('',#6455,1.3);
#2615=CIRCLE('',#6456,1.3);
#2616=CIRCLE('',#6459,1.24899959967968);
#2617=CIRCLE('',#6461,1.59980467557762);
#2618=CIRCLE('',#6469,0.275);
#2619=CIRCLE('',#6470,0.275);
#2620=CIRCLE('',#6472,0.275);
#2621=CIRCLE('',#6473,0.275);
#2622=CIRCLE('',#6475,0.275);
#2623=CIRCLE('',#6476,0.275);
#2624=CIRCLE('',#6478,0.275);
#2625=CIRCLE('',#6479,0.275);
#2626=CIRCLE('',#6485,1.6);
#2627=CIRCLE('',#6489,1.6);
#2628=CIRCLE('',#6496,1.2);
#2629=CIRCLE('',#6497,0.7);
#2630=CIRCLE('',#6499,1.2);
#2631=CIRCLE('',#6501,0.405);
#2632=CIRCLE('',#6503,0.405);
#2633=CIRCLE('',#6505,0.7);
#2634=CIRCLE('',#6509,0.1);
#2635=CIRCLE('',#6510,0.4);
#2636=CIRCLE('',#6513,0.61);
#2637=CIRCLE('',#6514,0.61);
#2638=CIRCLE('',#6516,0.405);
#2639=CIRCLE('',#6518,0.405);
#2640=CIRCLE('',#6520,1.);
#2641=CIRCLE('',#6521,1.);
#2642=CIRCLE('',#6526,0.3);
#2643=CIRCLE('',#6527,0.3);
#2644=CIRCLE('',#6530,0.3);
#2645=CIRCLE('',#6531,0.3);
#2646=CIRCLE('',#6534,0.225);
#2647=CIRCLE('',#6535,0.225);
#2648=CIRCLE('',#6537,0.225);
#2649=CIRCLE('',#6538,0.225);
#2650=CIRCLE('',#6540,0.225);
#2651=CIRCLE('',#6541,0.225);
#2652=CIRCLE('',#6543,0.225);
#2653=CIRCLE('',#6544,0.225);
#2654=CIRCLE('',#6546,1.01);
#2655=CIRCLE('',#6547,1.01);
#2656=CIRCLE('',#6556,1.11803398874989);
#2657=CIRCLE('',#6557,0.75);
#2658=CIRCLE('',#6559,0.75);
#2659=CIRCLE('',#6561,1.3);
#2660=CIRCLE('',#6562,1.3);
#2661=CIRCLE('',#6575,0.25);
#2662=CIRCLE('',#6576,0.24505);
#2663=CIRCLE('',#6578,0.25);
#2664=CIRCLE('',#6581,0.375);
#2665=CIRCLE('',#6583,0.425);
#2666=CIRCLE('',#6585,0.425);
#2667=CIRCLE('',#6587,0.395);
#2668=CIRCLE('',#6589,0.27);
#2669=CIRCLE('',#6591,0.24505);
#2670=CIRCLE('',#6595,0.285);
#2671=CIRCLE('',#6596,0.265);
#2672=CIRCLE('',#6598,0.265);
#2673=CIRCLE('',#6600,0.5);
#2674=CIRCLE('',#6602,0.5);
#2675=CIRCLE('',#6606,0.38);
#2676=CIRCLE('',#6608,0.38);
#2677=CIRCLE('',#6613,0.2117);
#2678=CIRCLE('',#6614,0.2117);
#2679=CIRCLE('',#6622,1.065);
#2680=CIRCLE('',#6624,1.065);
#2681=CIRCLE('',#6632,1.065);
#2682=CIRCLE('',#6634,0.985);
#2683=CIRCLE('',#6635,0.79);
#2684=CIRCLE('',#6638,1.065);
#2685=CIRCLE('',#6640,0.985);
#2686=CIRCLE('',#6642,0.79);
#2687=CIRCLE('',#6646,0.225);
#2688=CIRCLE('',#6647,0.225);
#2689=CIRCLE('',#6649,0.4);
#2690=CIRCLE('',#6650,0.4);
#2691=CIRCLE('',#6655,0.3);
#2692=CIRCLE('',#6657,0.35);
#2693=CIRCLE('',#6659,0.35);
#2694=CIRCLE('',#6661,0.32);
#2695=CIRCLE('',#6663,0.22);
#2696=CIRCLE('',#6665,0.1954);
#2697=CIRCLE('',#6667,0.1954);
#2698=CIRCLE('',#6669,0.16);
#2699=CIRCLE('',#6681,0.3);
#2700=CIRCLE('',#6682,0.3);
#2701=CIRCLE('',#6688,0.46);
#2702=CIRCLE('',#6689,0.46);
#2703=CIRCLE('',#6690,0.46);
#2704=CIRCLE('',#6692,0.513);
#2705=CIRCLE('',#6693,0.46);
#2706=CIRCLE('',#6694,0.46);
#2707=CIRCLE('',#6696,0.46);
#2708=CIRCLE('',#6698,0.57);
#2709=CIRCLE('',#6700,0.57);
#2710=CIRCLE('',#6702,0.57);
#2711=CIRCLE('',#6703,0.57);
#2712=CIRCLE('',#6706,0.825);
#2713=CIRCLE('',#6707,0.825);
#2714=CIRCLE('',#6708,0.825);
#2715=CIRCLE('',#6709,0.825);
#2716=CIRCLE('',#6712,0.825);
#2717=CIRCLE('',#6714,1.);
#2718=CIRCLE('',#6716,1.);
#2719=CIRCLE('',#6719,1.);
#2720=CIRCLE('',#6720,0.825);
#2721=CIRCLE('',#6722,1.);
#2722=CIRCLE('',#6727,0.685);
#2723=CIRCLE('',#6729,0.685);
#2724=CIRCLE('',#6737,0.685);
#2725=CIRCLE('',#6739,0.605);
#2726=CIRCLE('',#6740,0.46);
#2727=CIRCLE('',#6743,0.685);
#2728=CIRCLE('',#6745,0.605);
#2729=CIRCLE('',#6747,0.46);
#2730=CIRCLE('',#6751,0.2942);
#2731=CIRCLE('',#6752,0.2942);
#2732=CIRCLE('',#6754,0.24);
#2733=CIRCLE('',#6757,0.475);
#2734=CIRCLE('',#6816,1.48592563743951);
#2735=CIRCLE('',#6818,1.48592563743951);
#2736=CIRCLE('',#6819,1.48592563743951);
#2737=CIRCLE('',#6821,1.48592563743951);
#2738=CIRCLE('',#6823,1.48592563743951);
#2739=CIRCLE('',#6826,0.75);
#2740=CIRCLE('',#6827,0.75);
#2741=CIRCLE('',#6829,1.5);
#2742=CIRCLE('',#6832,0.165);
#2743=CIRCLE('',#6833,0.165);
#2744=CIRCLE('',#6836,0.4);
#2745=CIRCLE('',#6838,0.4);
#2746=CIRCLE('',#6840,0.4);
#2747=CIRCLE('',#6842,0.4);
#2748=CIRCLE('',#6849,0.4);
#2749=CIRCLE('',#6851,0.4);
#2750=CIRCLE('',#6852,0.4);
#2751=CIRCLE('',#6854,0.4);
#2752=CIRCLE('',#6856,0.4);
#2753=CIRCLE('',#6863,0.4);
#2754=CIRCLE('',#6878,0.225);
#2755=CIRCLE('',#6879,0.225);
#2756=CIRCLE('',#6881,0.6);
#2757=CIRCLE('',#6882,0.6);
#2758=CIRCLE('',#6902,0.1954);
#2759=CIRCLE('',#6904,0.3);
#2760=CIRCLE('',#6906,0.35);
#2761=CIRCLE('',#6908,0.35);
#2762=CIRCLE('',#6910,0.32);
#2763=CIRCLE('',#6912,0.22);
#2764=CIRCLE('',#6914,0.1954);
#2765=VERTEX_POINT('',#8770);
#2766=VERTEX_POINT('',#8772);
#2767=VERTEX_POINT('',#8776);
#2768=VERTEX_POINT('',#8779);
#2769=VERTEX_POINT('',#8781);
#2770=VERTEX_POINT('',#8785);
#2771=VERTEX_POINT('',#8790);
#2772=VERTEX_POINT('',#8792);
#2773=VERTEX_POINT('',#8799);
#2774=VERTEX_POINT('',#8801);
#2775=VERTEX_POINT('',#8805);
#2776=VERTEX_POINT('',#8808);
#2777=VERTEX_POINT('',#8810);
#2778=VERTEX_POINT('',#8814);
#2779=VERTEX_POINT('',#8819);
#2780=VERTEX_POINT('',#8821);
#2781=VERTEX_POINT('',#8828);
#2782=VERTEX_POINT('',#8830);
#2783=VERTEX_POINT('',#8834);
#2784=VERTEX_POINT('',#8836);
#2785=VERTEX_POINT('',#8840);
#2786=VERTEX_POINT('',#8842);
#2787=VERTEX_POINT('',#8846);
#2788=VERTEX_POINT('',#8848);
#2789=VERTEX_POINT('',#8852);
#2790=VERTEX_POINT('',#8854);
#2791=VERTEX_POINT('',#8858);
#2792=VERTEX_POINT('',#8860);
#2793=VERTEX_POINT('',#8865);
#2794=VERTEX_POINT('',#8867);
#2795=VERTEX_POINT('',#8872);
#2796=VERTEX_POINT('',#8874);
#2797=VERTEX_POINT('',#8878);
#2798=VERTEX_POINT('',#8879);
#2799=VERTEX_POINT('',#8881);
#2800=VERTEX_POINT('',#8883);
#2801=VERTEX_POINT('',#8887);
#2802=VERTEX_POINT('',#8888);
#2803=VERTEX_POINT('',#8890);
#2804=VERTEX_POINT('',#8892);
#2805=VERTEX_POINT('',#8896);
#2806=VERTEX_POINT('',#8898);
#2807=VERTEX_POINT('',#8900);
#2808=VERTEX_POINT('',#8902);
#2809=VERTEX_POINT('',#8909);
#2810=VERTEX_POINT('',#8913);
#2811=VERTEX_POINT('',#8914);
#2812=VERTEX_POINT('',#8921);
#2813=VERTEX_POINT('',#8927);
#2814=VERTEX_POINT('',#8929);
#2815=VERTEX_POINT('',#8934);
#2816=VERTEX_POINT('',#8936);
#2817=VERTEX_POINT('',#8940);
#2818=VERTEX_POINT('',#8941);
#2819=VERTEX_POINT('',#8943);
#2820=VERTEX_POINT('',#8945);
#2821=VERTEX_POINT('',#8949);
#2822=VERTEX_POINT('',#8950);
#2823=VERTEX_POINT('',#8952);
#2824=VERTEX_POINT('',#8954);
#2825=VERTEX_POINT('',#8958);
#2826=VERTEX_POINT('',#8960);
#2827=VERTEX_POINT('',#8962);
#2828=VERTEX_POINT('',#8964);
#2829=VERTEX_POINT('',#8971);
#2830=VERTEX_POINT('',#8975);
#2831=VERTEX_POINT('',#8976);
#2832=VERTEX_POINT('',#8983);
#2833=VERTEX_POINT('',#8989);
#2834=VERTEX_POINT('',#8990);
#2835=VERTEX_POINT('',#8992);
#2836=VERTEX_POINT('',#8994);
#2837=VERTEX_POINT('',#8998);
#2838=VERTEX_POINT('',#9000);
#2839=VERTEX_POINT('',#9004);
#2840=VERTEX_POINT('',#9006);
#2841=VERTEX_POINT('',#9016);
#2842=VERTEX_POINT('',#9018);
#2843=VERTEX_POINT('',#9022);
#2844=VERTEX_POINT('',#9023);
#2845=VERTEX_POINT('',#9025);
#2846=VERTEX_POINT('',#9027);
#2847=VERTEX_POINT('',#9031);
#2848=VERTEX_POINT('',#9033);
#2849=VERTEX_POINT('',#9037);
#2850=VERTEX_POINT('',#9039);
#2851=VERTEX_POINT('',#9043);
#2852=VERTEX_POINT('',#9045);
#2853=VERTEX_POINT('',#9049);
#2854=VERTEX_POINT('',#9051);
#2855=VERTEX_POINT('',#9061);
#2856=VERTEX_POINT('',#9063);
#2857=VERTEX_POINT('',#9066);
#2858=VERTEX_POINT('',#9070);
#2859=VERTEX_POINT('',#9073);
#2860=VERTEX_POINT('',#9077);
#2861=VERTEX_POINT('',#9081);
#2862=VERTEX_POINT('',#9084);
#2863=VERTEX_POINT('',#9088);
#2864=VERTEX_POINT('',#9092);
#2865=VERTEX_POINT('',#9095);
#2866=VERTEX_POINT('',#9099);
#2867=VERTEX_POINT('',#9103);
#2868=VERTEX_POINT('',#9104);
#2869=VERTEX_POINT('',#9106);
#2870=VERTEX_POINT('',#9108);
#2871=VERTEX_POINT('',#9110);
#2872=VERTEX_POINT('',#9112);
#2873=VERTEX_POINT('',#9115);
#2874=VERTEX_POINT('',#9118);
#2875=VERTEX_POINT('',#9120);
#2876=VERTEX_POINT('',#9124);
#2877=VERTEX_POINT('',#9128);
#2878=VERTEX_POINT('',#9132);
#2879=VERTEX_POINT('',#9136);
#2880=VERTEX_POINT('',#9143);
#2881=VERTEX_POINT('',#9149);
#2882=VERTEX_POINT('',#9151);
#2883=VERTEX_POINT('',#9156);
#2884=VERTEX_POINT('',#9158);
#2885=VERTEX_POINT('',#9163);
#2886=VERTEX_POINT('',#9165);
#2887=VERTEX_POINT('',#9169);
#2888=VERTEX_POINT('',#9171);
#2889=VERTEX_POINT('',#9175);
#2890=VERTEX_POINT('',#9177);
#2891=VERTEX_POINT('',#9181);
#2892=VERTEX_POINT('',#9183);
#2893=VERTEX_POINT('',#9187);
#2894=VERTEX_POINT('',#9188);
#2895=VERTEX_POINT('',#9190);
#2896=VERTEX_POINT('',#9192);
#2897=VERTEX_POINT('',#9196);
#2898=VERTEX_POINT('',#9198);
#2899=VERTEX_POINT('',#9202);
#2900=VERTEX_POINT('',#9204);
#2901=VERTEX_POINT('',#9206);
#2902=VERTEX_POINT('',#9208);
#2903=VERTEX_POINT('',#9212);
#2904=VERTEX_POINT('',#9214);
#2905=VERTEX_POINT('',#9218);
#2906=VERTEX_POINT('',#9220);
#2907=VERTEX_POINT('',#9224);
#2908=VERTEX_POINT('',#9230);
#2909=VERTEX_POINT('',#9232);
#2910=VERTEX_POINT('',#9236);
#2911=VERTEX_POINT('',#9240);
#2912=VERTEX_POINT('',#9248);
#2913=VERTEX_POINT('',#9250);
#2914=VERTEX_POINT('',#9255);
#2915=VERTEX_POINT('',#9257);
#2916=VERTEX_POINT('',#9262);
#2917=VERTEX_POINT('',#9264);
#2918=VERTEX_POINT('',#9268);
#2919=VERTEX_POINT('',#9270);
#2920=VERTEX_POINT('',#9274);
#2921=VERTEX_POINT('',#9276);
#2922=VERTEX_POINT('',#9280);
#2923=VERTEX_POINT('',#9282);
#2924=VERTEX_POINT('',#9286);
#2925=VERTEX_POINT('',#9287);
#2926=VERTEX_POINT('',#9289);
#2927=VERTEX_POINT('',#9291);
#2928=VERTEX_POINT('',#9295);
#2929=VERTEX_POINT('',#9297);
#2930=VERTEX_POINT('',#9301);
#2931=VERTEX_POINT('',#9303);
#2932=VERTEX_POINT('',#9305);
#2933=VERTEX_POINT('',#9307);
#2934=VERTEX_POINT('',#9311);
#2935=VERTEX_POINT('',#9313);
#2936=VERTEX_POINT('',#9317);
#2937=VERTEX_POINT('',#9319);
#2938=VERTEX_POINT('',#9324);
#2939=VERTEX_POINT('',#9329);
#2940=VERTEX_POINT('',#9330);
#2941=VERTEX_POINT('',#9335);
#2942=VERTEX_POINT('',#9339);
#2943=VERTEX_POINT('',#9347);
#2944=VERTEX_POINT('',#9349);
#2945=VERTEX_POINT('',#9353);
#2946=VERTEX_POINT('',#9355);
#2947=VERTEX_POINT('',#9359);
#2948=VERTEX_POINT('',#9361);
#2949=VERTEX_POINT('',#9365);
#2950=VERTEX_POINT('',#9367);
#2951=VERTEX_POINT('',#9371);
#2952=VERTEX_POINT('',#9372);
#2953=VERTEX_POINT('',#9374);
#2954=VERTEX_POINT('',#9376);
#2955=VERTEX_POINT('',#9380);
#2956=VERTEX_POINT('',#9381);
#2957=VERTEX_POINT('',#9383);
#2958=VERTEX_POINT('',#9385);
#2959=VERTEX_POINT('',#9389);
#2960=VERTEX_POINT('',#9391);
#2961=VERTEX_POINT('',#9395);
#2962=VERTEX_POINT('',#9397);
#2963=VERTEX_POINT('',#9402);
#2964=VERTEX_POINT('',#9404);
#2965=VERTEX_POINT('',#9406);
#2966=VERTEX_POINT('',#9408);
#2967=VERTEX_POINT('',#9412);
#2968=VERTEX_POINT('',#9416);
#2969=VERTEX_POINT('',#9422);
#2970=VERTEX_POINT('',#9426);
#2971=VERTEX_POINT('',#9434);
#2972=VERTEX_POINT('',#9436);
#2973=VERTEX_POINT('',#9439);
#2974=VERTEX_POINT('',#9443);
#2975=VERTEX_POINT('',#9446);
#2976=VERTEX_POINT('',#9450);
#2977=VERTEX_POINT('',#9456);
#2978=VERTEX_POINT('',#9461);
#2979=VERTEX_POINT('',#9463);
#2980=VERTEX_POINT('',#9467);
#2981=VERTEX_POINT('',#9470);
#2982=VERTEX_POINT('',#9474);
#2983=VERTEX_POINT('',#9476);
#2984=VERTEX_POINT('',#9483);
#2985=VERTEX_POINT('',#9485);
#2986=VERTEX_POINT('',#9490);
#2987=VERTEX_POINT('',#9492);
#2988=VERTEX_POINT('',#9497);
#2989=VERTEX_POINT('',#9499);
#2990=VERTEX_POINT('',#9503);
#2991=VERTEX_POINT('',#9505);
#2992=VERTEX_POINT('',#9509);
#2993=VERTEX_POINT('',#9511);
#2994=VERTEX_POINT('',#9515);
#2995=VERTEX_POINT('',#9517);
#2996=VERTEX_POINT('',#9521);
#2997=VERTEX_POINT('',#9523);
#2998=VERTEX_POINT('',#9527);
#2999=VERTEX_POINT('',#9528);
#3000=VERTEX_POINT('',#9530);
#3001=VERTEX_POINT('',#9532);
#3002=VERTEX_POINT('',#9536);
#3003=VERTEX_POINT('',#9538);
#3004=VERTEX_POINT('',#9542);
#3005=VERTEX_POINT('',#9544);
#3006=VERTEX_POINT('',#9554);
#3007=VERTEX_POINT('',#9556);
#3008=VERTEX_POINT('',#9559);
#3009=VERTEX_POINT('',#9563);
#3010=VERTEX_POINT('',#9565);
#3011=VERTEX_POINT('',#9572);
#3012=VERTEX_POINT('',#9573);
#3013=VERTEX_POINT('',#9575);
#3014=VERTEX_POINT('',#9577);
#3015=VERTEX_POINT('',#9581);
#3016=VERTEX_POINT('',#9583);
#3017=VERTEX_POINT('',#9587);
#3018=VERTEX_POINT('',#9589);
#3019=VERTEX_POINT('',#9593);
#3020=VERTEX_POINT('',#9595);
#3021=VERTEX_POINT('',#9599);
#3022=VERTEX_POINT('',#9601);
#3023=VERTEX_POINT('',#9610);
#3024=VERTEX_POINT('',#9612);
#3025=VERTEX_POINT('',#9615);
#3026=VERTEX_POINT('',#9620);
#3027=VERTEX_POINT('',#9623);
#3028=VERTEX_POINT('',#9627);
#3029=VERTEX_POINT('',#9631);
#3030=VERTEX_POINT('',#9635);
#3031=VERTEX_POINT('',#9638);
#3032=VERTEX_POINT('',#9645);
#3033=VERTEX_POINT('',#9647);
#3034=VERTEX_POINT('',#9651);
#3035=VERTEX_POINT('',#9655);
#3036=VERTEX_POINT('',#9658);
#3037=VERTEX_POINT('',#9664);
#3038=VERTEX_POINT('',#9665);
#3039=VERTEX_POINT('',#9669);
#3040=VERTEX_POINT('',#9673);
#3041=VERTEX_POINT('',#9676);
#3042=VERTEX_POINT('',#9680);
#3043=VERTEX_POINT('',#9684);
#3044=VERTEX_POINT('',#9692);
#3045=VERTEX_POINT('',#9694);
#3046=VERTEX_POINT('',#9696);
#3047=VERTEX_POINT('',#9700);
#3048=VERTEX_POINT('',#9704);
#3049=VERTEX_POINT('',#9708);
#3050=VERTEX_POINT('',#9712);
#3051=VERTEX_POINT('',#9727);
#3052=VERTEX_POINT('',#9729);
#3053=VERTEX_POINT('',#9741);
#3054=VERTEX_POINT('',#9742);
#3055=VERTEX_POINT('',#9744);
#3056=VERTEX_POINT('',#9746);
#3057=VERTEX_POINT('',#9748);
#3058=VERTEX_POINT('',#9750);
#3059=VERTEX_POINT('',#9753);
#3060=VERTEX_POINT('',#9756);
#3061=VERTEX_POINT('',#9757);
#3062=VERTEX_POINT('',#9759);
#3063=VERTEX_POINT('',#9761);
#3064=VERTEX_POINT('',#9763);
#3065=VERTEX_POINT('',#9765);
#3066=VERTEX_POINT('',#9768);
#3067=VERTEX_POINT('',#9783);
#3068=VERTEX_POINT('',#9787);
#3069=VERTEX_POINT('',#9789);
#3070=VERTEX_POINT('',#9794);
#3071=VERTEX_POINT('',#9798);
#3072=VERTEX_POINT('',#9802);
#3073=VERTEX_POINT('',#9808);
#3074=VERTEX_POINT('',#9810);
#3075=VERTEX_POINT('',#9814);
#3076=VERTEX_POINT('',#9816);
#3077=VERTEX_POINT('',#9823);
#3078=VERTEX_POINT('',#9826);
#3079=VERTEX_POINT('',#9830);
#3080=VERTEX_POINT('',#9834);
#3081=VERTEX_POINT('',#9838);
#3082=VERTEX_POINT('',#9841);
#3083=VERTEX_POINT('',#9845);
#3084=VERTEX_POINT('',#9849);
#3085=VERTEX_POINT('',#9854);
#3086=VERTEX_POINT('',#9855);
#3087=VERTEX_POINT('',#9857);
#3088=VERTEX_POINT('',#9859);
#3089=VERTEX_POINT('',#9863);
#3090=VERTEX_POINT('',#9865);
#3091=VERTEX_POINT('',#9869);
#3092=VERTEX_POINT('',#9871);
#3093=VERTEX_POINT('',#9875);
#3094=VERTEX_POINT('',#9877);
#3095=VERTEX_POINT('',#9881);
#3096=VERTEX_POINT('',#9883);
#3097=VERTEX_POINT('',#9893);
#3098=VERTEX_POINT('',#9895);
#3099=VERTEX_POINT('',#9902);
#3100=VERTEX_POINT('',#9903);
#3101=VERTEX_POINT('',#9905);
#3102=VERTEX_POINT('',#9907);
#3103=VERTEX_POINT('',#9912);
#3104=VERTEX_POINT('',#9913);
#3105=VERTEX_POINT('',#9915);
#3106=VERTEX_POINT('',#9919);
#3107=VERTEX_POINT('',#9923);
#3108=VERTEX_POINT('',#9926);
#3109=VERTEX_POINT('',#9930);
#3110=VERTEX_POINT('',#9932);
#3111=VERTEX_POINT('',#9937);
#3112=VERTEX_POINT('',#9938);
#3113=VERTEX_POINT('',#9940);
#3114=VERTEX_POINT('',#9942);
#3115=VERTEX_POINT('',#9947);
#3116=VERTEX_POINT('',#9951);
#3117=VERTEX_POINT('',#9954);
#3118=VERTEX_POINT('',#9959);
#3119=VERTEX_POINT('',#9961);
#3120=VERTEX_POINT('',#9964);
#3121=VERTEX_POINT('',#9972);
#3122=VERTEX_POINT('',#9973);
#3123=VERTEX_POINT('',#9975);
#3124=VERTEX_POINT('',#9977);
#3125=VERTEX_POINT('',#9979);
#3126=VERTEX_POINT('',#9981);
#3127=VERTEX_POINT('',#9984);
#3128=VERTEX_POINT('',#9987);
#3129=VERTEX_POINT('',#9988);
#3130=VERTEX_POINT('',#9990);
#3131=VERTEX_POINT('',#9992);
#3132=VERTEX_POINT('',#9994);
#3133=VERTEX_POINT('',#9996);
#3134=VERTEX_POINT('',#9999);
#3135=VERTEX_POINT('',#10014);
#3136=VERTEX_POINT('',#10018);
#3137=VERTEX_POINT('',#10020);
#3138=VERTEX_POINT('',#10025);
#3139=VERTEX_POINT('',#10029);
#3140=VERTEX_POINT('',#10033);
#3141=VERTEX_POINT('',#10039);
#3142=VERTEX_POINT('',#10041);
#3143=VERTEX_POINT('',#10045);
#3144=VERTEX_POINT('',#10050);
#3145=VERTEX_POINT('',#10052);
#3146=VERTEX_POINT('',#10054);
#3147=VERTEX_POINT('',#10058);
#3148=VERTEX_POINT('',#10062);
#3149=VERTEX_POINT('',#10066);
#3150=VERTEX_POINT('',#10070);
#3151=VERTEX_POINT('',#10078);
#3152=VERTEX_POINT('',#10080);
#3153=VERTEX_POINT('',#10084);
#3154=VERTEX_POINT('',#10088);
#3155=VERTEX_POINT('',#10092);
#3156=VERTEX_POINT('',#10096);
#3157=VERTEX_POINT('',#10153);
#3158=VERTEX_POINT('',#10154);
#3159=VERTEX_POINT('',#10156);
#3160=VERTEX_POINT('',#10158);
#3161=VERTEX_POINT('',#10162);
#3162=VERTEX_POINT('',#10164);
#3163=VERTEX_POINT('',#10166);
#3164=VERTEX_POINT('',#10170);
#3165=VERTEX_POINT('',#10172);
#3166=VERTEX_POINT('',#10180);
#3167=VERTEX_POINT('',#10182);
#3168=VERTEX_POINT('',#10186);
#3169=VERTEX_POINT('',#10190);
#3170=VERTEX_POINT('',#10192);
#3171=VERTEX_POINT('',#10197);
#3172=VERTEX_POINT('',#10198);
#3173=VERTEX_POINT('',#10200);
#3174=VERTEX_POINT('',#10204);
#3175=VERTEX_POINT('',#10205);
#3176=VERTEX_POINT('',#10207);
#3177=VERTEX_POINT('',#10211);
#3178=VERTEX_POINT('',#10212);
#3179=VERTEX_POINT('',#10214);
#3180=VERTEX_POINT('',#10218);
#3181=VERTEX_POINT('',#10219);
#3182=VERTEX_POINT('',#10221);
#3183=VERTEX_POINT('',#10226);
#3184=VERTEX_POINT('',#10228);
#3185=VERTEX_POINT('',#10233);
#3186=VERTEX_POINT('',#10238);
#3187=VERTEX_POINT('',#10248);
#3188=VERTEX_POINT('',#10256);
#3189=VERTEX_POINT('',#10257);
#3190=VERTEX_POINT('',#10259);
#3191=VERTEX_POINT('',#10261);
#3192=VERTEX_POINT('',#10265);
#3193=VERTEX_POINT('',#10267);
#3194=VERTEX_POINT('',#10271);
#3195=VERTEX_POINT('',#10273);
#3196=VERTEX_POINT('',#10281);
#3197=VERTEX_POINT('',#10287);
#3198=VERTEX_POINT('',#10288);
#3199=VERTEX_POINT('',#10290);
#3200=VERTEX_POINT('',#10292);
#3201=VERTEX_POINT('',#10296);
#3202=VERTEX_POINT('',#10298);
#3203=VERTEX_POINT('',#10302);
#3204=VERTEX_POINT('',#10304);
#3205=VERTEX_POINT('',#10311);
#3206=VERTEX_POINT('',#10312);
#3207=VERTEX_POINT('',#10314);
#3208=VERTEX_POINT('',#10316);
#3209=VERTEX_POINT('',#10320);
#3210=VERTEX_POINT('',#10322);
#3211=VERTEX_POINT('',#10326);
#3212=VERTEX_POINT('',#10328);
#3213=VERTEX_POINT('',#10338);
#3214=VERTEX_POINT('',#10340);
#3215=VERTEX_POINT('',#10344);
#3216=VERTEX_POINT('',#10346);
#3217=VERTEX_POINT('',#10353);
#3218=VERTEX_POINT('',#10354);
#3219=VERTEX_POINT('',#10356);
#3220=VERTEX_POINT('',#10358);
#3221=VERTEX_POINT('',#10362);
#3222=VERTEX_POINT('',#10364);
#3223=VERTEX_POINT('',#10368);
#3224=VERTEX_POINT('',#10370);
#3225=VERTEX_POINT('',#10380);
#3226=VERTEX_POINT('',#10381);
#3227=VERTEX_POINT('',#10383);
#3228=VERTEX_POINT('',#10385);
#3229=VERTEX_POINT('',#10389);
#3230=VERTEX_POINT('',#10391);
#3231=VERTEX_POINT('',#10395);
#3232=VERTEX_POINT('',#10397);
#3233=VERTEX_POINT('',#10401);
#3234=VERTEX_POINT('',#10403);
#3235=VERTEX_POINT('',#10407);
#3236=VERTEX_POINT('',#10409);
#3237=VERTEX_POINT('',#10418);
#3238=VERTEX_POINT('',#10421);
#3239=VERTEX_POINT('',#10424);
#3240=VERTEX_POINT('',#10428);
#3241=VERTEX_POINT('',#10432);
#3242=VERTEX_POINT('',#10436);
#3243=VERTEX_POINT('',#10439);
#3244=EDGE_CURVE('',#2765,#2765,#2520,.T.);
#3245=EDGE_CURVE('',#2765,#2766,#1592,.T.);
#3246=EDGE_CURVE('',#2766,#2766,#2521,.T.);
#3247=EDGE_CURVE('',#2767,#2767,#2522,.T.);
#3248=EDGE_CURVE('',#2768,#2768,#2523,.T.);
#3249=EDGE_CURVE('',#2768,#2769,#1593,.T.);
#3250=EDGE_CURVE('',#2769,#2769,#2524,.T.);
#3251=EDGE_CURVE('',#2770,#2770,#2525,.T.);
#3252=EDGE_CURVE('',#2770,#2767,#1594,.T.);
#3253=EDGE_CURVE('',#2771,#2771,#2526,.T.);
#3254=EDGE_CURVE('',#2771,#2772,#1595,.T.);
#3255=EDGE_CURVE('',#2772,#2772,#2527,.T.);
#3256=EDGE_CURVE('',#2773,#2773,#2528,.T.);
#3257=EDGE_CURVE('',#2773,#2774,#1596,.T.);
#3258=EDGE_CURVE('',#2774,#2774,#2529,.T.);
#3259=EDGE_CURVE('',#2775,#2775,#2530,.T.);
#3260=EDGE_CURVE('',#2776,#2776,#2531,.T.);
#3261=EDGE_CURVE('',#2776,#2777,#1597,.T.);
#3262=EDGE_CURVE('',#2777,#2777,#2532,.T.);
#3263=EDGE_CURVE('',#2778,#2778,#2533,.T.);
#3264=EDGE_CURVE('',#2775,#2778,#1598,.T.);
#3265=EDGE_CURVE('',#2779,#2779,#2534,.T.);
#3266=EDGE_CURVE('',#2779,#2780,#1599,.T.);
#3267=EDGE_CURVE('',#2780,#2780,#2535,.T.);
#3268=EDGE_CURVE('',#2781,#2781,#2536,.T.);
#3269=EDGE_CURVE('',#2781,#2782,#1600,.T.);
#3270=EDGE_CURVE('',#2782,#2782,#2537,.T.);
#3271=EDGE_CURVE('',#2783,#2783,#2538,.T.);
#3272=EDGE_CURVE('',#2783,#2784,#1601,.T.);
#3273=EDGE_CURVE('',#2784,#2784,#2539,.T.);
#3274=EDGE_CURVE('',#2785,#2785,#2540,.T.);
#3275=EDGE_CURVE('',#2785,#2786,#1602,.T.);
#3276=EDGE_CURVE('',#2786,#2786,#2541,.T.);
#3277=EDGE_CURVE('',#2787,#2787,#2542,.T.);
#3278=EDGE_CURVE('',#2787,#2788,#1603,.T.);
#3279=EDGE_CURVE('',#2788,#2788,#2543,.T.);
#3280=EDGE_CURVE('',#2789,#2789,#2544,.T.);
#3281=EDGE_CURVE('',#2789,#2790,#1604,.T.);
#3282=EDGE_CURVE('',#2790,#2790,#2545,.T.);
#3283=EDGE_CURVE('',#2791,#2791,#2546,.T.);
#3284=EDGE_CURVE('',#2791,#2792,#1605,.T.);
#3285=EDGE_CURVE('',#2792,#2792,#2547,.T.);
#3286=EDGE_CURVE('',#2793,#2793,#2548,.T.);
#3287=EDGE_CURVE('',#2793,#2794,#1606,.T.);
#3288=EDGE_CURVE('',#2794,#2794,#2549,.T.);
#3289=EDGE_CURVE('',#2795,#2795,#2550,.T.);
#3290=EDGE_CURVE('',#2795,#2796,#1607,.T.);
#3291=EDGE_CURVE('',#2796,#2796,#2551,.T.);
#3292=EDGE_CURVE('',#2797,#2798,#1608,.T.);
#3293=EDGE_CURVE('',#2799,#2797,#1609,.T.);
#3294=EDGE_CURVE('',#2800,#2799,#1610,.T.);
#3295=EDGE_CURVE('',#2798,#2800,#1611,.T.);
#3296=EDGE_CURVE('',#2801,#2802,#1612,.T.);
#3297=EDGE_CURVE('',#2803,#2801,#1613,.T.);
#3298=EDGE_CURVE('',#2804,#2803,#1614,.T.);
#3299=EDGE_CURVE('',#2802,#2804,#1615,.T.);
#3300=EDGE_CURVE('',#2797,#2805,#1616,.T.);
#3301=EDGE_CURVE('',#2805,#2806,#1617,.T.);
#3302=EDGE_CURVE('',#2807,#2806,#1618,.T.);
#3303=EDGE_CURVE('',#2807,#2808,#1619,.T.);
#3304=EDGE_CURVE('',#2808,#2802,#1620,.T.);
#3305=EDGE_CURVE('',#2804,#2799,#2552,.T.);
#3306=EDGE_CURVE('',#2800,#2803,#2553,.T.);
#3307=EDGE_CURVE('',#2809,#2808,#1621,.T.);
#3308=EDGE_CURVE('',#2801,#2809,#1622,.T.);
#3309=EDGE_CURVE('',#2810,#2811,#1623,.T.);
#3310=EDGE_CURVE('',#2806,#2810,#1624,.T.);
#3311=EDGE_CURVE('',#2811,#2805,#1625,.T.);
#3312=EDGE_CURVE('',#2811,#2798,#1626,.T.);
#3313=EDGE_CURVE('',#2809,#2812,#1627,.T.);
#3314=EDGE_CURVE('',#2812,#2807,#1628,.T.);
#3315=EDGE_CURVE('',#2810,#2812,#1629,.T.);
#3316=EDGE_CURVE('',#2813,#2813,#2554,.T.);
#3317=EDGE_CURVE('',#2813,#2814,#1630,.T.);
#3318=EDGE_CURVE('',#2814,#2814,#2555,.T.);
#3319=EDGE_CURVE('',#2815,#2815,#2556,.T.);
#3320=EDGE_CURVE('',#2815,#2816,#1631,.T.);
#3321=EDGE_CURVE('',#2816,#2816,#2557,.T.);
#3322=EDGE_CURVE('',#2817,#2818,#1632,.T.);
#3323=EDGE_CURVE('',#2819,#2817,#1633,.T.);
#3324=EDGE_CURVE('',#2820,#2819,#1634,.T.);
#3325=EDGE_CURVE('',#2818,#2820,#1635,.T.);
#3326=EDGE_CURVE('',#2821,#2822,#1636,.T.);
#3327=EDGE_CURVE('',#2823,#2821,#1637,.T.);
#3328=EDGE_CURVE('',#2824,#2823,#1638,.T.);
#3329=EDGE_CURVE('',#2822,#2824,#1639,.T.);
#3330=EDGE_CURVE('',#2817,#2825,#1640,.T.);
#3331=EDGE_CURVE('',#2825,#2826,#1641,.T.);
#3332=EDGE_CURVE('',#2827,#2826,#1642,.T.);
#3333=EDGE_CURVE('',#2827,#2828,#1643,.T.);
#3334=EDGE_CURVE('',#2828,#2822,#1644,.T.);
#3335=EDGE_CURVE('',#2824,#2819,#2558,.T.);
#3336=EDGE_CURVE('',#2820,#2823,#2559,.T.);
#3337=EDGE_CURVE('',#2829,#2828,#1645,.T.);
#3338=EDGE_CURVE('',#2821,#2829,#1646,.T.);
#3339=EDGE_CURVE('',#2830,#2831,#1647,.T.);
#3340=EDGE_CURVE('',#2826,#2830,#1648,.T.);
#3341=EDGE_CURVE('',#2831,#2825,#1649,.T.);
#3342=EDGE_CURVE('',#2831,#2818,#1650,.T.);
#3343=EDGE_CURVE('',#2829,#2832,#1651,.T.);
#3344=EDGE_CURVE('',#2832,#2827,#1652,.T.);
#3345=EDGE_CURVE('',#2830,#2832,#1653,.T.);
#3346=EDGE_CURVE('',#2833,#2834,#1654,.T.);
#3347=EDGE_CURVE('',#2834,#2835,#1655,.T.);
#3348=EDGE_CURVE('',#2836,#2835,#1656,.T.);
#3349=EDGE_CURVE('',#2833,#2836,#1657,.T.);
#3350=EDGE_CURVE('',#2837,#2833,#1658,.T.);
#3351=EDGE_CURVE('',#2838,#2836,#1659,.T.);
#3352=EDGE_CURVE('',#2837,#2838,#1660,.T.);
#3353=EDGE_CURVE('',#2839,#2837,#1661,.T.);
#3354=EDGE_CURVE('',#2840,#2838,#1662,.T.);
#3355=EDGE_CURVE('',#2839,#2840,#1663,.T.);
#3356=EDGE_CURVE('',#2834,#2839,#1664,.T.);
#3357=EDGE_CURVE('',#2835,#2840,#1665,.T.);
#3358=EDGE_CURVE('',#2841,#2841,#2560,.T.);
#3359=EDGE_CURVE('',#2841,#2842,#1666,.T.);
#3360=EDGE_CURVE('',#2842,#2842,#2561,.T.);
#3361=EDGE_CURVE('',#2843,#2844,#1667,.T.);
#3362=EDGE_CURVE('',#2844,#2845,#1668,.T.);
#3363=EDGE_CURVE('',#2846,#2845,#1669,.T.);
#3364=EDGE_CURVE('',#2843,#2846,#1670,.T.);
#3365=EDGE_CURVE('',#2847,#2843,#1671,.T.);
#3366=EDGE_CURVE('',#2848,#2846,#1672,.T.);
#3367=EDGE_CURVE('',#2847,#2848,#1673,.T.);
#3368=EDGE_CURVE('',#2849,#2847,#1674,.T.);
#3369=EDGE_CURVE('',#2850,#2848,#1675,.T.);
#3370=EDGE_CURVE('',#2849,#2850,#1676,.T.);
#3371=EDGE_CURVE('',#2851,#2849,#1677,.T.);
#3372=EDGE_CURVE('',#2852,#2850,#1678,.T.);
#3373=EDGE_CURVE('',#2851,#2852,#1679,.T.);
#3374=EDGE_CURVE('',#2853,#2851,#1680,.T.);
#3375=EDGE_CURVE('',#2854,#2852,#1681,.T.);
#3376=EDGE_CURVE('',#2853,#2854,#1682,.T.);
#3377=EDGE_CURVE('',#2844,#2853,#1683,.T.);
#3378=EDGE_CURVE('',#2845,#2854,#1684,.T.);
#3379=EDGE_CURVE('',#2855,#2855,#2562,.T.);
#3380=EDGE_CURVE('',#2856,#2856,#2563,.T.);
#3381=EDGE_CURVE('',#2857,#2857,#2564,.T.);
#3382=EDGE_CURVE('',#2857,#2855,#1685,.T.);
#3383=EDGE_CURVE('',#2858,#2858,#2565,.T.);
#3384=EDGE_CURVE('',#2859,#2859,#2566,.T.);
#3385=EDGE_CURVE('',#2859,#2858,#1686,.T.);
#3386=EDGE_CURVE('',#2860,#2860,#2567,.T.);
#3387=EDGE_CURVE('',#2860,#2859,#1687,.T.);
#3388=EDGE_CURVE('',#2861,#2861,#2568,.T.);
#3389=EDGE_CURVE('',#2862,#2862,#2569,.T.);
#3390=EDGE_CURVE('',#2862,#2861,#1688,.T.);
#3391=EDGE_CURVE('',#2863,#2863,#2570,.T.);
#3392=EDGE_CURVE('',#2863,#2862,#1689,.T.);
#3393=EDGE_CURVE('',#2864,#2864,#2571,.T.);
#3394=EDGE_CURVE('',#2865,#2865,#2572,.T.);
#3395=EDGE_CURVE('',#2865,#2864,#1690,.T.);
#3396=EDGE_CURVE('',#2866,#2866,#2573,.T.);
#3397=EDGE_CURVE('',#2866,#2856,#1691,.T.);
#3398=EDGE_CURVE('',#2867,#2868,#1692,.T.);
#3399=EDGE_CURVE('',#2868,#2869,#1693,.T.);
#3400=EDGE_CURVE('',#2869,#2870,#1694,.T.);
#3401=EDGE_CURVE('',#2870,#2871,#1695,.T.);
#3402=EDGE_CURVE('',#2871,#2872,#1696,.T.);
#3403=EDGE_CURVE('',#2872,#2867,#1697,.T.);
#3404=EDGE_CURVE('',#2873,#2873,#2574,.T.);
#3405=EDGE_CURVE('',#2868,#2874,#1698,.T.);
#3406=EDGE_CURVE('',#2875,#2874,#1699,.T.);
#3407=EDGE_CURVE('',#2869,#2875,#1700,.T.);
#3408=EDGE_CURVE('',#2876,#2875,#1701,.T.);
#3409=EDGE_CURVE('',#2870,#2876,#1702,.T.);
#3410=EDGE_CURVE('',#2877,#2876,#1703,.T.);
#3411=EDGE_CURVE('',#2871,#2877,#1704,.T.);
#3412=EDGE_CURVE('',#2878,#2877,#1705,.T.);
#3413=EDGE_CURVE('',#2872,#2878,#1706,.T.);
#3414=EDGE_CURVE('',#2879,#2878,#1707,.T.);
#3415=EDGE_CURVE('',#2867,#2879,#1708,.T.);
#3416=EDGE_CURVE('',#2874,#2879,#1709,.T.);
#3417=EDGE_CURVE('',#2873,#2880,#1710,.T.);
#3418=EDGE_CURVE('',#2880,#2880,#2575,.T.);
#3419=EDGE_CURVE('',#2881,#2881,#2576,.T.);
#3420=EDGE_CURVE('',#2881,#2882,#1711,.T.);
#3421=EDGE_CURVE('',#2882,#2882,#2577,.T.);
#3422=EDGE_CURVE('',#2883,#2883,#2578,.T.);
#3423=EDGE_CURVE('',#2883,#2884,#1712,.T.);
#3424=EDGE_CURVE('',#2884,#2884,#2579,.T.);
#3425=EDGE_CURVE('',#2885,#2885,#2580,.T.);
#3426=EDGE_CURVE('',#2885,#2886,#1713,.T.);
#3427=EDGE_CURVE('',#2886,#2886,#2581,.T.);
#3428=EDGE_CURVE('',#2887,#2887,#2582,.T.);
#3429=EDGE_CURVE('',#2887,#2888,#1714,.T.);
#3430=EDGE_CURVE('',#2888,#2888,#2583,.T.);
#3431=EDGE_CURVE('',#2889,#2889,#2584,.T.);
#3432=EDGE_CURVE('',#2889,#2890,#1715,.T.);
#3433=EDGE_CURVE('',#2890,#2890,#2585,.T.);
#3434=EDGE_CURVE('',#2891,#2891,#2586,.T.);
#3435=EDGE_CURVE('',#2891,#2892,#1716,.T.);
#3436=EDGE_CURVE('',#2892,#2892,#2587,.T.);
#3437=EDGE_CURVE('',#2893,#2894,#1717,.T.);
#3438=EDGE_CURVE('',#2895,#2893,#2588,.T.);
#3439=EDGE_CURVE('',#2896,#2895,#1718,.T.);
#3440=EDGE_CURVE('',#2894,#2896,#2589,.T.);
#3441=EDGE_CURVE('',#2897,#2893,#1719,.T.);
#3442=EDGE_CURVE('',#2898,#2897,#2590,.T.);
#3443=EDGE_CURVE('',#2895,#2898,#1720,.T.);
#3444=EDGE_CURVE('',#2896,#2899,#1721,.T.);
#3445=EDGE_CURVE('',#2899,#2900,#1722,.T.);
#3446=EDGE_CURVE('',#2900,#2901,#1723,.T.);
#3447=EDGE_CURVE('',#2901,#2902,#1724,.T.);
#3448=EDGE_CURVE('',#2902,#2894,#1725,.T.);
#3449=EDGE_CURVE('',#2903,#2903,#2591,.T.);
#3450=EDGE_CURVE('',#2903,#2904,#1726,.T.);
#3451=EDGE_CURVE('',#2904,#2904,#2592,.T.);
#3452=EDGE_CURVE('',#2905,#2905,#2593,.T.);
#3453=EDGE_CURVE('',#2905,#2906,#1727,.T.);
#3454=EDGE_CURVE('',#2906,#2906,#2594,.T.);
#3455=EDGE_CURVE('',#2907,#2907,#2595,.T.);
#3456=EDGE_CURVE('',#2898,#2897,#2596,.T.);
#3457=EDGE_CURVE('',#2908,#2902,#1728,.T.);
#3458=EDGE_CURVE('',#2908,#2909,#1729,.T.);
#3459=EDGE_CURVE('',#2909,#2899,#1730,.T.);
#3460=EDGE_CURVE('',#2910,#2908,#1731,.T.);
#3461=EDGE_CURVE('',#2910,#2901,#1732,.T.);
#3462=EDGE_CURVE('',#2911,#2910,#1733,.T.);
#3463=EDGE_CURVE('',#2911,#2900,#1734,.T.);
#3464=EDGE_CURVE('',#2909,#2911,#1735,.T.);
#3465=EDGE_CURVE('',#2912,#2912,#2597,.T.);
#3466=EDGE_CURVE('',#2912,#2913,#1736,.T.);
#3467=EDGE_CURVE('',#2913,#2913,#2598,.T.);
#3468=EDGE_CURVE('',#2914,#2914,#2599,.T.);
#3469=EDGE_CURVE('',#2914,#2915,#1737,.T.);
#3470=EDGE_CURVE('',#2915,#2915,#2600,.T.);
#3471=EDGE_CURVE('',#2916,#2916,#2601,.T.);
#3472=EDGE_CURVE('',#2916,#2917,#1738,.T.);
#3473=EDGE_CURVE('',#2917,#2917,#2602,.T.);
#3474=EDGE_CURVE('',#2918,#2918,#2603,.T.);
#3475=EDGE_CURVE('',#2918,#2919,#1739,.T.);
#3476=EDGE_CURVE('',#2919,#2919,#2604,.T.);
#3477=EDGE_CURVE('',#2920,#2920,#2605,.T.);
#3478=EDGE_CURVE('',#2920,#2921,#1740,.T.);
#3479=EDGE_CURVE('',#2921,#2921,#2606,.T.);
#3480=EDGE_CURVE('',#2922,#2922,#2607,.T.);
#3481=EDGE_CURVE('',#2922,#2923,#1741,.T.);
#3482=EDGE_CURVE('',#2923,#2923,#2608,.T.);
#3483=EDGE_CURVE('',#2924,#2925,#1742,.T.);
#3484=EDGE_CURVE('',#2926,#2924,#2609,.T.);
#3485=EDGE_CURVE('',#2927,#2926,#1743,.T.);
#3486=EDGE_CURVE('',#2925,#2927,#2610,.T.);
#3487=EDGE_CURVE('',#2928,#2924,#1744,.T.);
#3488=EDGE_CURVE('',#2929,#2928,#2611,.T.);
#3489=EDGE_CURVE('',#2926,#2929,#1745,.T.);
#3490=EDGE_CURVE('',#2927,#2930,#1746,.T.);
#3491=EDGE_CURVE('',#2930,#2931,#1747,.T.);
#3492=EDGE_CURVE('',#2931,#2932,#1748,.T.);
#3493=EDGE_CURVE('',#2932,#2933,#1749,.T.);
#3494=EDGE_CURVE('',#2933,#2925,#1750,.T.);
#3495=EDGE_CURVE('',#2934,#2934,#2612,.T.);
#3496=EDGE_CURVE('',#2934,#2935,#1751,.T.);
#3497=EDGE_CURVE('',#2935,#2935,#2613,.T.);
#3498=EDGE_CURVE('',#2936,#2936,#2614,.T.);
#3499=EDGE_CURVE('',#2936,#2937,#1752,.T.);
#3500=EDGE_CURVE('',#2937,#2937,#2615,.T.);
#3501=EDGE_CURVE('',#2938,#2938,#2616,.T.);
#3502=EDGE_CURVE('',#2929,#2928,#2617,.T.);
#3503=EDGE_CURVE('',#2939,#2940,#1753,.T.);
#3504=EDGE_CURVE('',#2940,#2932,#1754,.T.);
#3505=EDGE_CURVE('',#2939,#2931,#1755,.T.);
#3506=EDGE_CURVE('',#2941,#2939,#1756,.T.);
#3507=EDGE_CURVE('',#2941,#2930,#1757,.T.);
#3508=EDGE_CURVE('',#2942,#2933,#1758,.T.);
#3509=EDGE_CURVE('',#2942,#2941,#1759,.T.);
#3510=EDGE_CURVE('',#2940,#2942,#1760,.T.);
#3511=EDGE_CURVE('',#2943,#2943,#2618,.T.);
#3512=EDGE_CURVE('',#2943,#2944,#1761,.T.);
#3513=EDGE_CURVE('',#2944,#2944,#2619,.T.);
#3514=EDGE_CURVE('',#2945,#2945,#2620,.T.);
#3515=EDGE_CURVE('',#2945,#2946,#1762,.T.);
#3516=EDGE_CURVE('',#2946,#2946,#2621,.T.);
#3517=EDGE_CURVE('',#2947,#2947,#2622,.T.);
#3518=EDGE_CURVE('',#2947,#2948,#1763,.T.);
#3519=EDGE_CURVE('',#2948,#2948,#2623,.T.);
#3520=EDGE_CURVE('',#2949,#2949,#2624,.T.);
#3521=EDGE_CURVE('',#2949,#2950,#1764,.T.);
#3522=EDGE_CURVE('',#2950,#2950,#2625,.T.);
#3523=EDGE_CURVE('',#2951,#2952,#1765,.T.);
#3524=EDGE_CURVE('',#2951,#2953,#1766,.T.);
#3525=EDGE_CURVE('',#2954,#2953,#1767,.T.);
#3526=EDGE_CURVE('',#2952,#2954,#1768,.T.);
#3527=EDGE_CURVE('',#2955,#2956,#1769,.T.);
#3528=EDGE_CURVE('',#2955,#2957,#1770,.T.);
#3529=EDGE_CURVE('',#2958,#2957,#1771,.T.);
#3530=EDGE_CURVE('',#2956,#2958,#1772,.T.);
#3531=EDGE_CURVE('',#2959,#2951,#1773,.T.);
#3532=EDGE_CURVE('',#2960,#2959,#1774,.T.);
#3533=EDGE_CURVE('',#2953,#2960,#1775,.T.);
#3534=EDGE_CURVE('',#2961,#2955,#1776,.T.);
#3535=EDGE_CURVE('',#2962,#2961,#1777,.T.);
#3536=EDGE_CURVE('',#2957,#2962,#1778,.T.);
#3537=EDGE_CURVE('',#2960,#2958,#2626,.T.);
#3538=EDGE_CURVE('',#2962,#2963,#1779,.T.);
#3539=EDGE_CURVE('',#2963,#2964,#1780,.T.);
#3540=EDGE_CURVE('',#2964,#2965,#1781,.T.);
#3541=EDGE_CURVE('',#2965,#2966,#1782,.T.);
#3542=EDGE_CURVE('',#2966,#2954,#1783,.T.);
#3543=EDGE_CURVE('',#2967,#2961,#1784,.T.);
#3544=EDGE_CURVE('',#2967,#2963,#1785,.T.);
#3545=EDGE_CURVE('',#2968,#2966,#1786,.T.);
#3546=EDGE_CURVE('',#2952,#2968,#1787,.T.);
#3547=EDGE_CURVE('',#2956,#2959,#2627,.T.);
#3548=EDGE_CURVE('',#2968,#2969,#1788,.T.);
#3549=EDGE_CURVE('',#2969,#2965,#1789,.T.);
#3550=EDGE_CURVE('',#2969,#2970,#1790,.T.);
#3551=EDGE_CURVE('',#2970,#2964,#1791,.T.);
#3552=EDGE_CURVE('',#2970,#2967,#1792,.T.);
#3553=EDGE_CURVE('',#2971,#2971,#2628,.T.);
#3554=EDGE_CURVE('',#2972,#2972,#2629,.T.);
#3555=EDGE_CURVE('',#2973,#2973,#2630,.T.);
#3556=EDGE_CURVE('',#2973,#2971,#1793,.T.);
#3557=EDGE_CURVE('',#2974,#2974,#2631,.T.);
#3558=EDGE_CURVE('',#2974,#2975,#1794,.T.);
#3559=EDGE_CURVE('',#2975,#2975,#2632,.T.);
#3560=EDGE_CURVE('',#2972,#2976,#1795,.T.);
#3561=EDGE_CURVE('',#2976,#2976,#2633,.T.);
#3562=EDGE_CURVE('',#2977,#2977,#2634,.T.);
#3563=EDGE_CURVE('',#2977,#2977,#2635,.T.);
#3564=EDGE_CURVE('',#2978,#2978,#2636,.T.);
#3565=EDGE_CURVE('',#2978,#2979,#1796,.T.);
#3566=EDGE_CURVE('',#2979,#2979,#2637,.T.);
#3567=EDGE_CURVE('',#2980,#2980,#2638,.T.);
#3568=EDGE_CURVE('',#2981,#2981,#2639,.T.);
#3569=EDGE_CURVE('',#2981,#2980,#1797,.T.);
#3570=EDGE_CURVE('',#2982,#2982,#2640,.T.);
#3571=EDGE_CURVE('',#2982,#2983,#1798,.T.);
#3572=EDGE_CURVE('',#2983,#2983,#2641,.T.);
#3573=EDGE_CURVE('',#2984,#2984,#2642,.T.);
#3574=EDGE_CURVE('',#2984,#2985,#1799,.T.);
#3575=EDGE_CURVE('',#2985,#2985,#2643,.T.);
#3576=EDGE_CURVE('',#2986,#2986,#2644,.T.);
#3577=EDGE_CURVE('',#2986,#2987,#1800,.T.);
#3578=EDGE_CURVE('',#2987,#2987,#2645,.T.);
#3579=EDGE_CURVE('',#2988,#2988,#2646,.T.);
#3580=EDGE_CURVE('',#2988,#2989,#1801,.T.);
#3581=EDGE_CURVE('',#2989,#2989,#2647,.T.);
#3582=EDGE_CURVE('',#2990,#2990,#2648,.T.);
#3583=EDGE_CURVE('',#2990,#2991,#1802,.T.);
#3584=EDGE_CURVE('',#2991,#2991,#2649,.T.);
#3585=EDGE_CURVE('',#2992,#2992,#2650,.T.);
#3586=EDGE_CURVE('',#2992,#2993,#1803,.T.);
#3587=EDGE_CURVE('',#2993,#2993,#2651,.T.);
#3588=EDGE_CURVE('',#2994,#2994,#2652,.T.);
#3589=EDGE_CURVE('',#2994,#2995,#1804,.T.);
#3590=EDGE_CURVE('',#2995,#2995,#2653,.T.);
#3591=EDGE_CURVE('',#2996,#2996,#2654,.T.);
#3592=EDGE_CURVE('',#2996,#2997,#1805,.T.);
#3593=EDGE_CURVE('',#2997,#2997,#2655,.T.);
#3594=EDGE_CURVE('',#2998,#2999,#1806,.T.);
#3595=EDGE_CURVE('',#2999,#3000,#1807,.T.);
#3596=EDGE_CURVE('',#3001,#3000,#1808,.T.);
#3597=EDGE_CURVE('',#2998,#3001,#1809,.T.);
#3598=EDGE_CURVE('',#3002,#2998,#1810,.T.);
#3599=EDGE_CURVE('',#3003,#3001,#1811,.T.);
#3600=EDGE_CURVE('',#3002,#3003,#1812,.T.);
#3601=EDGE_CURVE('',#3004,#3002,#1813,.T.);
#3602=EDGE_CURVE('',#3005,#3003,#1814,.T.);
#3603=EDGE_CURVE('',#3004,#3005,#1815,.T.);
#3604=EDGE_CURVE('',#2999,#3004,#1816,.T.);
#3605=EDGE_CURVE('',#3000,#3005,#1817,.T.);
#3606=EDGE_CURVE('',#3006,#3006,#2656,.T.);
#3607=EDGE_CURVE('',#3007,#3007,#2657,.T.);
#3608=EDGE_CURVE('',#3007,#3008,#1818,.T.);
#3609=EDGE_CURVE('',#3008,#3008,#2658,.T.);
#3610=EDGE_CURVE('',#3009,#3009,#2659,.T.);
#3611=EDGE_CURVE('',#3009,#3010,#1819,.T.);
#3612=EDGE_CURVE('',#3010,#3010,#2660,.T.);
#3613=EDGE_CURVE('',#3011,#3012,#1820,.T.);
#3614=EDGE_CURVE('',#3012,#3013,#1821,.T.);
#3615=EDGE_CURVE('',#3013,#3014,#1822,.T.);
#3616=EDGE_CURVE('',#3011,#3014,#1823,.T.);
#3617=EDGE_CURVE('',#3012,#3015,#1824,.T.);
#3618=EDGE_CURVE('',#3015,#3016,#1825,.T.);
#3619=EDGE_CURVE('',#3016,#3013,#1826,.T.);
#3620=EDGE_CURVE('',#3015,#3017,#1827,.T.);
#3621=EDGE_CURVE('',#3017,#3018,#1828,.T.);
#3622=EDGE_CURVE('',#3018,#3016,#1829,.T.);
#3623=EDGE_CURVE('',#3017,#3019,#1830,.T.);
#3624=EDGE_CURVE('',#3019,#3020,#1831,.T.);
#3625=EDGE_CURVE('',#3020,#3018,#1832,.T.);
#3626=EDGE_CURVE('',#3019,#3021,#1833,.T.);
#3627=EDGE_CURVE('',#3021,#3022,#1834,.T.);
#3628=EDGE_CURVE('',#3022,#3020,#1835,.T.);
#3629=EDGE_CURVE('',#3021,#3011,#1836,.T.);
#3630=EDGE_CURVE('',#3014,#3022,#1837,.T.);
#3631=EDGE_CURVE('',#3023,#3023,#2661,.T.);
#3632=EDGE_CURVE('',#3024,#3024,#2662,.T.);
#3633=EDGE_CURVE('',#3023,#3025,#1838,.T.);
#3634=EDGE_CURVE('',#3025,#3025,#2663,.T.);
#3635=EDGE_CURVE('',#3026,#3026,#2664,.T.);
#3636=EDGE_CURVE('',#3027,#3027,#2665,.T.);
#3637=EDGE_CURVE('',#3027,#3026,#1839,.T.);
#3638=EDGE_CURVE('',#3028,#3028,#2666,.T.);
#3639=EDGE_CURVE('',#3028,#3027,#1840,.T.);
#3640=EDGE_CURVE('',#3029,#3029,#2667,.T.);
#3641=EDGE_CURVE('',#3029,#3028,#1841,.T.);
#3642=EDGE_CURVE('',#3030,#3030,#2668,.T.);
#3643=EDGE_CURVE('',#3031,#3031,#2669,.F.);
#3644=EDGE_CURVE('',#3031,#3030,#1842,.T.);
#3645=EDGE_CURVE('',#3024,#3031,#1843,.T.);
#3646=EDGE_CURVE('',#3032,#3032,#2670,.T.);
#3647=EDGE_CURVE('',#3032,#3033,#1844,.T.);
#3648=EDGE_CURVE('',#3033,#3033,#2671,.T.);
#3649=EDGE_CURVE('',#3033,#3034,#1845,.T.);
#3650=EDGE_CURVE('',#3034,#3034,#2672,.T.);
#3651=EDGE_CURVE('',#3035,#3035,#2673,.T.);
#3652=EDGE_CURVE('',#3035,#3036,#1846,.T.);
#3653=EDGE_CURVE('',#3036,#3036,#2674,.T.);
#3654=EDGE_CURVE('',#3037,#3038,#233,.T.);
#3655=EDGE_CURVE('',#3039,#3037,#234,.T.);
#3656=EDGE_CURVE('',#3039,#3040,#1847,.T.);
#3657=EDGE_CURVE('',#3040,#3040,#2675,.T.);
#3658=EDGE_CURVE('',#3041,#3039,#235,.T.);
#3659=EDGE_CURVE('',#3042,#3041,#236,.T.);
#3660=EDGE_CURVE('',#3043,#3042,#237,.T.);
#3661=EDGE_CURVE('',#3038,#3043,#238,.T.);
#3662=EDGE_CURVE('',#3044,#3044,#2676,.T.);
#3663=EDGE_CURVE('',#3044,#3045,#1848,.T.);
#3664=EDGE_CURVE('',#3046,#3045,#239,.T.);
#3665=EDGE_CURVE('',#3047,#3046,#240,.T.);
#3666=EDGE_CURVE('',#3048,#3047,#241,.T.);
#3667=EDGE_CURVE('',#3049,#3048,#242,.T.);
#3668=EDGE_CURVE('',#3050,#3049,#243,.T.);
#3669=EDGE_CURVE('',#3045,#3050,#244,.T.);
#3670=EDGE_CURVE('',#3041,#3050,#1849,.T.);
#3671=EDGE_CURVE('',#3042,#3049,#1850,.T.);
#3672=EDGE_CURVE('',#3039,#3045,#1851,.T.);
#3673=EDGE_CURVE('',#3037,#3046,#1852,.T.);
#3674=EDGE_CURVE('',#3051,#3051,#2677,.F.);
#3675=EDGE_CURVE('',#3051,#3052,#1853,.T.);
#3676=EDGE_CURVE('',#3052,#3052,#2678,.F.);
#3677=EDGE_CURVE('',#3038,#3047,#1854,.T.);
#3678=EDGE_CURVE('',#3043,#3048,#1855,.T.);
#3679=EDGE_CURVE('',#3053,#3054,#1856,.T.);
#3680=EDGE_CURVE('',#3054,#3055,#1857,.T.);
#3681=EDGE_CURVE('',#3055,#3056,#1858,.T.);
#3682=EDGE_CURVE('',#3056,#3057,#1859,.T.);
#3683=EDGE_CURVE('',#3057,#3058,#1860,.T.);
#3684=EDGE_CURVE('',#3058,#3053,#1861,.T.);
#3685=EDGE_CURVE('',#3059,#3059,#2679,.T.);
#3686=EDGE_CURVE('',#3060,#3061,#1862,.T.);
#3687=EDGE_CURVE('',#3061,#3062,#1863,.T.);
#3688=EDGE_CURVE('',#3062,#3063,#1864,.T.);
#3689=EDGE_CURVE('',#3063,#3064,#1865,.T.);
#3690=EDGE_CURVE('',#3064,#3065,#1866,.T.);
#3691=EDGE_CURVE('',#3065,#3060,#1867,.T.);
#3692=EDGE_CURVE('',#3066,#3066,#2680,.T.);
#3693=EDGE_CURVE('',#3060,#3054,#1868,.T.);
#3694=EDGE_CURVE('',#3055,#3065,#1869,.T.);
#3695=EDGE_CURVE('',#3056,#3064,#1870,.T.);
#3696=EDGE_CURVE('',#3057,#3063,#1871,.T.);
#3697=EDGE_CURVE('',#3058,#3062,#1872,.T.);
#3698=EDGE_CURVE('',#3053,#3061,#1873,.T.);
#3699=EDGE_CURVE('',#3066,#3067,#1874,.T.);
#3700=EDGE_CURVE('',#3067,#3067,#2681,.T.);
#3701=EDGE_CURVE('',#3068,#3068,#2682,.T.);
#3702=EDGE_CURVE('',#3069,#3069,#2683,.T.);
#3703=EDGE_CURVE('',#3067,#3068,#1875,.T.);
#3704=EDGE_CURVE('',#3070,#3070,#2684,.T.);
#3705=EDGE_CURVE('',#3070,#3059,#1876,.T.);
#3706=EDGE_CURVE('',#3071,#3071,#2685,.T.);
#3707=EDGE_CURVE('',#3071,#3070,#1877,.T.);
#3708=EDGE_CURVE('',#3072,#3072,#2686,.T.);
#3709=EDGE_CURVE('',#3072,#3069,#1878,.T.);
#3710=EDGE_CURVE('',#3073,#3073,#2687,.T.);
#3711=EDGE_CURVE('',#3073,#3074,#1879,.T.);
#3712=EDGE_CURVE('',#3074,#3074,#2688,.T.);
#3713=EDGE_CURVE('',#3075,#3075,#2689,.T.);
#3714=EDGE_CURVE('',#3075,#3076,#1880,.T.);
#3715=EDGE_CURVE('',#3076,#3076,#2690,.T.);
#3716=EDGE_CURVE('',#3077,#3077,#2691,.T.);
#3717=EDGE_CURVE('',#3078,#3078,#2692,.T.);
#3718=EDGE_CURVE('',#3078,#3077,#1881,.T.);
#3719=EDGE_CURVE('',#3079,#3079,#2693,.T.);
#3720=EDGE_CURVE('',#3079,#3078,#1882,.T.);
#3721=EDGE_CURVE('',#3080,#3080,#2694,.T.);
#3722=EDGE_CURVE('',#3080,#3079,#1883,.T.);
#3723=EDGE_CURVE('',#3081,#3081,#2695,.T.);
#3724=EDGE_CURVE('',#3082,#3082,#2696,.F.);
#3725=EDGE_CURVE('',#3082,#3081,#1884,.T.);
#3726=EDGE_CURVE('',#3083,#3083,#2697,.F.);
#3727=EDGE_CURVE('',#3083,#3082,#1885,.T.);
#3728=EDGE_CURVE('',#3084,#3084,#2698,.T.);
#3729=EDGE_CURVE('',#3084,#3083,#1886,.T.);
#3730=EDGE_CURVE('',#3085,#3086,#1887,.T.);
#3731=EDGE_CURVE('',#3086,#3087,#1888,.T.);
#3732=EDGE_CURVE('',#3087,#3088,#1889,.T.);
#3733=EDGE_CURVE('',#3085,#3088,#1890,.T.);
#3734=EDGE_CURVE('',#3086,#3089,#1891,.T.);
#3735=EDGE_CURVE('',#3089,#3090,#1892,.T.);
#3736=EDGE_CURVE('',#3090,#3087,#1893,.T.);
#3737=EDGE_CURVE('',#3089,#3091,#1894,.T.);
#3738=EDGE_CURVE('',#3091,#3092,#1895,.T.);
#3739=EDGE_CURVE('',#3092,#3090,#1896,.T.);
#3740=EDGE_CURVE('',#3091,#3093,#1897,.T.);
#3741=EDGE_CURVE('',#3093,#3094,#1898,.T.);
#3742=EDGE_CURVE('',#3094,#3092,#1899,.T.);
#3743=EDGE_CURVE('',#3093,#3095,#1900,.T.);
#3744=EDGE_CURVE('',#3095,#3096,#1901,.T.);
#3745=EDGE_CURVE('',#3096,#3094,#1902,.T.);
#3746=EDGE_CURVE('',#3095,#3085,#1903,.T.);
#3747=EDGE_CURVE('',#3088,#3096,#1904,.T.);
#3748=EDGE_CURVE('',#3097,#3097,#2699,.T.);
#3749=EDGE_CURVE('',#3097,#3098,#1905,.T.);
#3750=EDGE_CURVE('',#3098,#3098,#2700,.T.);
#3751=EDGE_CURVE('',#3099,#3100,#231,.T.);
#3752=EDGE_CURVE('',#3101,#3099,#2701,.T.);
#3753=EDGE_CURVE('',#3101,#3102,#1906,.T.);
#3754=EDGE_CURVE('',#3102,#3102,#2702,.T.);
#3755=EDGE_CURVE('',#3100,#3101,#2703,.T.);
#3756=EDGE_CURVE('',#3103,#3104,#2704,.T.);
#3757=EDGE_CURVE('',#3099,#3105,#2705,.T.);
#3758=EDGE_CURVE('',#3105,#3100,#2706,.T.);
#3759=EDGE_CURVE('',#3105,#3106,#1907,.T.);
#3760=EDGE_CURVE('',#3106,#3106,#2707,.T.);
#3761=EDGE_CURVE('',#3107,#3107,#2708,.T.);
#3762=EDGE_CURVE('',#3108,#3108,#2709,.T.);
#3763=EDGE_CURVE('',#3108,#3107,#1908,.T.);
#3764=EDGE_CURVE('',#3109,#3109,#2710,.T.);
#3765=EDGE_CURVE('',#3109,#3110,#1909,.T.);
#3766=EDGE_CURVE('',#3110,#3110,#2711,.T.);
#3767=EDGE_CURVE('',#3111,#3112,#2712,.T.);
#3768=EDGE_CURVE('',#3112,#3113,#2713,.T.);
#3769=EDGE_CURVE('',#3114,#3113,#2714,.T.);
#3770=EDGE_CURVE('',#3111,#3114,#2715,.T.);
#3771=EDGE_CURVE('',#3113,#3111,#232,.T.);
#3772=EDGE_CURVE('',#3112,#3115,#1910,.T.);
#3773=EDGE_CURVE('',#3115,#3115,#2716,.T.);
#3774=EDGE_CURVE('',#3116,#3116,#2717,.T.);
#3775=EDGE_CURVE('',#3117,#3117,#2718,.T.);
#3776=EDGE_CURVE('',#3117,#3116,#1911,.T.);
#3777=EDGE_CURVE('',#3118,#3118,#2719,.T.);
#3778=EDGE_CURVE('',#3119,#3119,#2720,.T.);
#3779=EDGE_CURVE('',#3120,#3120,#2721,.T.);
#3780=EDGE_CURVE('',#3120,#3118,#1912,.T.);
#3781=EDGE_CURVE('',#3119,#3114,#1913,.T.);
#3782=EDGE_CURVE('',#3121,#3122,#1914,.T.);
#3783=EDGE_CURVE('',#3122,#3123,#1915,.T.);
#3784=EDGE_CURVE('',#3123,#3124,#1916,.T.);
#3785=EDGE_CURVE('',#3124,#3125,#1917,.T.);
#3786=EDGE_CURVE('',#3125,#3126,#1918,.T.);
#3787=EDGE_CURVE('',#3126,#3121,#1919,.T.);
#3788=EDGE_CURVE('',#3127,#3127,#2722,.T.);
#3789=EDGE_CURVE('',#3128,#3129,#1920,.T.);
#3790=EDGE_CURVE('',#3129,#3130,#1921,.T.);
#3791=EDGE_CURVE('',#3130,#3131,#1922,.T.);
#3792=EDGE_CURVE('',#3131,#3132,#1923,.T.);
#3793=EDGE_CURVE('',#3132,#3133,#1924,.T.);
#3794=EDGE_CURVE('',#3133,#3128,#1925,.T.);
#3795=EDGE_CURVE('',#3134,#3134,#2723,.T.);
#3796=EDGE_CURVE('',#3128,#3122,#1926,.T.);
#3797=EDGE_CURVE('',#3123,#3133,#1927,.T.);
#3798=EDGE_CURVE('',#3124,#3132,#1928,.T.);
#3799=EDGE_CURVE('',#3125,#3131,#1929,.T.);
#3800=EDGE_CURVE('',#3126,#3130,#1930,.T.);
#3801=EDGE_CURVE('',#3121,#3129,#1931,.T.);
#3802=EDGE_CURVE('',#3134,#3135,#1932,.T.);
#3803=EDGE_CURVE('',#3135,#3135,#2724,.T.);
#3804=EDGE_CURVE('',#3136,#3136,#2725,.T.);
#3805=EDGE_CURVE('',#3137,#3137,#2726,.T.);
#3806=EDGE_CURVE('',#3135,#3136,#1933,.T.);
#3807=EDGE_CURVE('',#3138,#3138,#2727,.T.);
#3808=EDGE_CURVE('',#3138,#3127,#1934,.T.);
#3809=EDGE_CURVE('',#3139,#3139,#2728,.T.);
#3810=EDGE_CURVE('',#3139,#3138,#1935,.T.);
#3811=EDGE_CURVE('',#3140,#3140,#2729,.T.);
#3812=EDGE_CURVE('',#3140,#3137,#1936,.T.);
#3813=EDGE_CURVE('',#3141,#3141,#2730,.F.);
#3814=EDGE_CURVE('',#3141,#3142,#1937,.T.);
#3815=EDGE_CURVE('',#3142,#3142,#2731,.F.);
#3816=EDGE_CURVE('',#3143,#3143,#2732,.T.);
#3817=EDGE_CURVE('',#3143,#3141,#1938,.T.);
#3818=EDGE_CURVE('',#3144,#3144,#2733,.T.);
#3819=EDGE_CURVE('',#3144,#3145,#1939,.T.);
#3820=EDGE_CURVE('',#3146,#3145,#245,.T.);
#3821=EDGE_CURVE('',#3147,#3146,#246,.T.);
#3822=EDGE_CURVE('',#3148,#3147,#247,.T.);
#3823=EDGE_CURVE('',#3149,#3148,#248,.T.);
#3824=EDGE_CURVE('',#3150,#3149,#249,.T.);
#3825=EDGE_CURVE('',#3145,#3150,#250,.T.);
#3826=EDGE_CURVE('',#3151,#3149,#1940,.T.);
#3827=EDGE_CURVE('',#3151,#3152,#1941,.T.);
#3828=EDGE_CURVE('',#3152,#3150,#1942,.T.);
#3829=EDGE_CURVE('',#3153,#3148,#1943,.T.);
#3830=EDGE_CURVE('',#3153,#3151,#1944,.T.);
#3831=EDGE_CURVE('',#3154,#3147,#1945,.T.);
#3832=EDGE_CURVE('',#3154,#3153,#1946,.T.);
#3833=EDGE_CURVE('',#3155,#3146,#1947,.T.);
#3834=EDGE_CURVE('',#3155,#3154,#1948,.T.);
#3835=EDGE_CURVE('',#3156,#3145,#1949,.T.);
#3836=EDGE_CURVE('',#3156,#3155,#1950,.T.);
#3837=EDGE_CURVE('',#3152,#3156,#1951,.T.);
#3838=EDGE_CURVE('',#3157,#3158,#2734,.T.);
#3839=EDGE_CURVE('',#3159,#3157,#1952,.T.);
#3840=EDGE_CURVE('',#3160,#3159,#1953,.T.);
#3841=EDGE_CURVE('',#3160,#3158,#1954,.T.);
#3842=EDGE_CURVE('',#3158,#3161,#2735,.T.);
#3843=EDGE_CURVE('',#3162,#3160,#1955,.T.);
#3844=EDGE_CURVE('',#3162,#3163,#1956,.T.);
#3845=EDGE_CURVE('',#3161,#3163,#2736,.T.);
#3846=EDGE_CURVE('',#3163,#3164,#2737,.T.);
#3847=EDGE_CURVE('',#3165,#3162,#1957,.T.);
#3848=EDGE_CURVE('',#3165,#3164,#1958,.T.);
#3849=EDGE_CURVE('',#3164,#3157,#2738,.T.);
#3850=EDGE_CURVE('',#3159,#3165,#1959,.T.);
#3851=EDGE_CURVE('',#3166,#3166,#2739,.T.);
#3852=EDGE_CURVE('',#3166,#3167,#1960,.T.);
#3853=EDGE_CURVE('',#3167,#3167,#2740,.T.);
#3854=EDGE_CURVE('',#3161,#3168,#2741,.T.);
#3855=EDGE_CURVE('',#3169,#3169,#2742,.T.);
#3856=EDGE_CURVE('',#3169,#3170,#1961,.T.);
#3857=EDGE_CURVE('',#3170,#3170,#2743,.T.);
#3858=EDGE_CURVE('',#3171,#3172,#2744,.T.);
#3859=EDGE_CURVE('',#3173,#3172,#1962,.T.);
#3860=EDGE_CURVE('',#3171,#3173,#1963,.T.);
#3861=EDGE_CURVE('',#3174,#3175,#2745,.T.);
#3862=EDGE_CURVE('',#3176,#3175,#1964,.T.);
#3863=EDGE_CURVE('',#3174,#3176,#1965,.T.);
#3864=EDGE_CURVE('',#3177,#3178,#2746,.T.);
#3865=EDGE_CURVE('',#3179,#3178,#1966,.T.);
#3866=EDGE_CURVE('',#3177,#3179,#1967,.T.);
#3867=EDGE_CURVE('',#3180,#3181,#2747,.T.);
#3868=EDGE_CURVE('',#3182,#3181,#1968,.T.);
#3869=EDGE_CURVE('',#3180,#3182,#1969,.T.);
#3870=EDGE_CURVE('',#3171,#3181,#1970,.T.);
#3871=EDGE_CURVE('',#3173,#3183,#1971,.T.);
#3872=EDGE_CURVE('',#3184,#3183,#1972,.T.);
#3873=EDGE_CURVE('',#3182,#3184,#1973,.T.);
#3874=EDGE_CURVE('',#3180,#3178,#1974,.T.);
#3875=EDGE_CURVE('',#3185,#3184,#1975,.T.);
#3876=EDGE_CURVE('',#3179,#3185,#1976,.T.);
#3877=EDGE_CURVE('',#3177,#3175,#1977,.T.);
#3878=EDGE_CURVE('',#3186,#3185,#1978,.T.);
#3879=EDGE_CURVE('',#3176,#3186,#1979,.T.);
#3880=EDGE_CURVE('',#3174,#3172,#1980,.T.);
#3881=EDGE_CURVE('',#3183,#3186,#1981,.T.);
#3882=EDGE_CURVE('',#3175,#3177,#2748,.T.);
#3883=EDGE_CURVE('',#3172,#3187,#2749,.T.);
#3884=EDGE_CURVE('',#3187,#3174,#2750,.T.);
#3885=EDGE_CURVE('',#3181,#3171,#2751,.T.);
#3886=EDGE_CURVE('',#3178,#3180,#2752,.T.);
#3887=EDGE_CURVE('',#3188,#3189,#1982,.T.);
#3888=EDGE_CURVE('',#3189,#3190,#1983,.T.);
#3889=EDGE_CURVE('',#3191,#3190,#1984,.T.);
#3890=EDGE_CURVE('',#3188,#3191,#1985,.T.);
#3891=EDGE_CURVE('',#3192,#3188,#1986,.T.);
#3892=EDGE_CURVE('',#3193,#3191,#1987,.T.);
#3893=EDGE_CURVE('',#3192,#3193,#1988,.T.);
#3894=EDGE_CURVE('',#3194,#3192,#1989,.T.);
#3895=EDGE_CURVE('',#3195,#3193,#1990,.T.);
#3896=EDGE_CURVE('',#3194,#3195,#1991,.T.);
#3897=EDGE_CURVE('',#3189,#3194,#1992,.T.);
#3898=EDGE_CURVE('',#3190,#3195,#1993,.T.);
#3899=EDGE_CURVE('',#3187,#3196,#1994,.T.);
#3900=EDGE_CURVE('',#3196,#3196,#2753,.T.);
#3901=EDGE_CURVE('',#3197,#3198,#1995,.T.);
#3902=EDGE_CURVE('',#3199,#3197,#1996,.T.);
#3903=EDGE_CURVE('',#3200,#3199,#1997,.T.);
#3904=EDGE_CURVE('',#3200,#3198,#1998,.T.);
#3905=EDGE_CURVE('',#3198,#3201,#1999,.T.);
#3906=EDGE_CURVE('',#3202,#3200,#2000,.T.);
#3907=EDGE_CURVE('',#3202,#3201,#2001,.T.);
#3908=EDGE_CURVE('',#3201,#3203,#2002,.T.);
#3909=EDGE_CURVE('',#3204,#3202,#2003,.T.);
#3910=EDGE_CURVE('',#3204,#3203,#2004,.T.);
#3911=EDGE_CURVE('',#3203,#3197,#2005,.T.);
#3912=EDGE_CURVE('',#3199,#3204,#2006,.T.);
#3913=EDGE_CURVE('',#3205,#3206,#2007,.T.);
#3914=EDGE_CURVE('',#3206,#3207,#2008,.T.);
#3915=EDGE_CURVE('',#3208,#3207,#2009,.T.);
#3916=EDGE_CURVE('',#3205,#3208,#2010,.T.);
#3917=EDGE_CURVE('',#3209,#3205,#2011,.T.);
#3918=EDGE_CURVE('',#3210,#3208,#2012,.T.);
#3919=EDGE_CURVE('',#3209,#3210,#2013,.T.);
#3920=EDGE_CURVE('',#3211,#3209,#2014,.T.);
#3921=EDGE_CURVE('',#3212,#3210,#2015,.T.);
#3922=EDGE_CURVE('',#3211,#3212,#2016,.T.);
#3923=EDGE_CURVE('',#3206,#3211,#2017,.T.);
#3924=EDGE_CURVE('',#3207,#3212,#2018,.T.);
#3925=EDGE_CURVE('',#3213,#3213,#2754,.T.);
#3926=EDGE_CURVE('',#3213,#3214,#2019,.T.);
#3927=EDGE_CURVE('',#3214,#3214,#2755,.T.);
#3928=EDGE_CURVE('',#3215,#3215,#2756,.T.);
#3929=EDGE_CURVE('',#3215,#3216,#2020,.T.);
#3930=EDGE_CURVE('',#3216,#3216,#2757,.T.);
#3931=EDGE_CURVE('',#3217,#3218,#2021,.T.);
#3932=EDGE_CURVE('',#3218,#3219,#2022,.T.);
#3933=EDGE_CURVE('',#3220,#3219,#2023,.T.);
#3934=EDGE_CURVE('',#3217,#3220,#2024,.T.);
#3935=EDGE_CURVE('',#3221,#3217,#2025,.T.);
#3936=EDGE_CURVE('',#3222,#3220,#2026,.T.);
#3937=EDGE_CURVE('',#3221,#3222,#2027,.T.);
#3938=EDGE_CURVE('',#3223,#3221,#2028,.T.);
#3939=EDGE_CURVE('',#3224,#3222,#2029,.T.);
#3940=EDGE_CURVE('',#3223,#3224,#2030,.T.);
#3941=EDGE_CURVE('',#3218,#3223,#2031,.T.);
#3942=EDGE_CURVE('',#3219,#3224,#2032,.T.);
#3943=EDGE_CURVE('',#3225,#3226,#2033,.T.);
#3944=EDGE_CURVE('',#3226,#3227,#2034,.T.);
#3945=EDGE_CURVE('',#3227,#3228,#2035,.T.);
#3946=EDGE_CURVE('',#3225,#3228,#2036,.T.);
#3947=EDGE_CURVE('',#3226,#3229,#2037,.T.);
#3948=EDGE_CURVE('',#3229,#3230,#2038,.T.);
#3949=EDGE_CURVE('',#3230,#3227,#2039,.T.);
#3950=EDGE_CURVE('',#3229,#3231,#2040,.T.);
#3951=EDGE_CURVE('',#3231,#3232,#2041,.T.);
#3952=EDGE_CURVE('',#3232,#3230,#2042,.T.);
#3953=EDGE_CURVE('',#3231,#3233,#2043,.T.);
#3954=EDGE_CURVE('',#3233,#3234,#2044,.T.);
#3955=EDGE_CURVE('',#3234,#3232,#2045,.T.);
#3956=EDGE_CURVE('',#3233,#3235,#2046,.T.);
#3957=EDGE_CURVE('',#3235,#3236,#2047,.T.);
#3958=EDGE_CURVE('',#3236,#3234,#2048,.T.);
#3959=EDGE_CURVE('',#3235,#3225,#2049,.T.);
#3960=EDGE_CURVE('',#3228,#3236,#2050,.T.);
#3961=EDGE_CURVE('',#3237,#3237,#2758,.T.);
#3962=EDGE_CURVE('',#3238,#3238,#2759,.T.);
#3963=EDGE_CURVE('',#3239,#3239,#2760,.T.);
#3964=EDGE_CURVE('',#3239,#3238,#2051,.T.);
#3965=EDGE_CURVE('',#3240,#3240,#2761,.T.);
#3966=EDGE_CURVE('',#3240,#3239,#2052,.T.);
#3967=EDGE_CURVE('',#3241,#3241,#2762,.T.);
#3968=EDGE_CURVE('',#3241,#3240,#2053,.T.);
#3969=EDGE_CURVE('',#3242,#3242,#2763,.T.);
#3970=EDGE_CURVE('',#3243,#3243,#2764,.F.);
#3971=EDGE_CURVE('',#3243,#3242,#2054,.T.);
#3972=EDGE_CURVE('',#3237,#3243,#2055,.T.);
#3973=ORIENTED_EDGE('',*,*,#3244,.F.);
#3974=ORIENTED_EDGE('',*,*,#3245,.T.);
#3975=ORIENTED_EDGE('',*,*,#3246,.T.);
#3976=ORIENTED_EDGE('',*,*,#3245,.F.);
#3977=ORIENTED_EDGE('',*,*,#3246,.F.);
#3978=ORIENTED_EDGE('',*,*,#3247,.F.);
#3979=ORIENTED_EDGE('',*,*,#3248,.F.);
#3980=ORIENTED_EDGE('',*,*,#3249,.T.);
#3981=ORIENTED_EDGE('',*,*,#3250,.F.);
#3982=ORIENTED_EDGE('',*,*,#3249,.F.);
#3983=ORIENTED_EDGE('',*,*,#3248,.T.);
#3984=ORIENTED_EDGE('',*,*,#3251,.F.);
#3985=ORIENTED_EDGE('',*,*,#3251,.T.);
#3986=ORIENTED_EDGE('',*,*,#3252,.T.);
#3987=ORIENTED_EDGE('',*,*,#3247,.T.);
#3988=ORIENTED_EDGE('',*,*,#3252,.F.);
#3989=ORIENTED_EDGE('',*,*,#3253,.F.);
#3990=ORIENTED_EDGE('',*,*,#3254,.T.);
#3991=ORIENTED_EDGE('',*,*,#3255,.T.);
#3992=ORIENTED_EDGE('',*,*,#3254,.F.);
#3993=ORIENTED_EDGE('',*,*,#3253,.T.);
#3994=ORIENTED_EDGE('',*,*,#3250,.T.);
#3995=ORIENTED_EDGE('',*,*,#3255,.F.);
#3996=ORIENTED_EDGE('',*,*,#3244,.T.);
#3997=ORIENTED_EDGE('',*,*,#3256,.F.);
#3998=ORIENTED_EDGE('',*,*,#3257,.T.);
#3999=ORIENTED_EDGE('',*,*,#3258,.F.);
#4000=ORIENTED_EDGE('',*,*,#3257,.F.);
#4001=ORIENTED_EDGE('',*,*,#3256,.T.);
#4002=ORIENTED_EDGE('',*,*,#3259,.F.);
#4003=ORIENTED_EDGE('',*,*,#3260,.F.);
#4004=ORIENTED_EDGE('',*,*,#3261,.T.);
#4005=ORIENTED_EDGE('',*,*,#3262,.T.);
#4006=ORIENTED_EDGE('',*,*,#3261,.F.);
#4007=ORIENTED_EDGE('',*,*,#3262,.F.);
#4008=ORIENTED_EDGE('',*,*,#3263,.F.);
#4009=ORIENTED_EDGE('',*,*,#3259,.T.);
#4010=ORIENTED_EDGE('',*,*,#3264,.T.);
#4011=ORIENTED_EDGE('',*,*,#3263,.T.);
#4012=ORIENTED_EDGE('',*,*,#3264,.F.);
#4013=ORIENTED_EDGE('',*,*,#3265,.F.);
#4014=ORIENTED_EDGE('',*,*,#3266,.T.);
#4015=ORIENTED_EDGE('',*,*,#3267,.T.);
#4016=ORIENTED_EDGE('',*,*,#3266,.F.);
#4017=ORIENTED_EDGE('',*,*,#3265,.T.);
#4018=ORIENTED_EDGE('',*,*,#3258,.T.);
#4019=ORIENTED_EDGE('',*,*,#3267,.F.);
#4020=ORIENTED_EDGE('',*,*,#3260,.T.);
#4021=ORIENTED_EDGE('',*,*,#3268,.F.);
#4022=ORIENTED_EDGE('',*,*,#3269,.T.);
#4023=ORIENTED_EDGE('',*,*,#3270,.F.);
#4024=ORIENTED_EDGE('',*,*,#3269,.F.);
#4025=ORIENTED_EDGE('',*,*,#3271,.F.);
#4026=ORIENTED_EDGE('',*,*,#3272,.T.);
#4027=ORIENTED_EDGE('',*,*,#3273,.F.);
#4028=ORIENTED_EDGE('',*,*,#3272,.F.);
#4029=ORIENTED_EDGE('',*,*,#3274,.F.);
#4030=ORIENTED_EDGE('',*,*,#3275,.T.);
#4031=ORIENTED_EDGE('',*,*,#3276,.F.);
#4032=ORIENTED_EDGE('',*,*,#3275,.F.);
#4033=ORIENTED_EDGE('',*,*,#3277,.F.);
#4034=ORIENTED_EDGE('',*,*,#3278,.T.);
#4035=ORIENTED_EDGE('',*,*,#3279,.F.);
#4036=ORIENTED_EDGE('',*,*,#3278,.F.);
#4037=ORIENTED_EDGE('',*,*,#3280,.F.);
#4038=ORIENTED_EDGE('',*,*,#3281,.T.);
#4039=ORIENTED_EDGE('',*,*,#3282,.F.);
#4040=ORIENTED_EDGE('',*,*,#3281,.F.);
#4041=ORIENTED_EDGE('',*,*,#3283,.F.);
#4042=ORIENTED_EDGE('',*,*,#3284,.T.);
#4043=ORIENTED_EDGE('',*,*,#3285,.F.);
#4044=ORIENTED_EDGE('',*,*,#3284,.F.);
#4045=ORIENTED_EDGE('',*,*,#3283,.T.);
#4046=ORIENTED_EDGE('',*,*,#3282,.T.);
#4047=ORIENTED_EDGE('',*,*,#3286,.F.);
#4048=ORIENTED_EDGE('',*,*,#3287,.T.);
#4049=ORIENTED_EDGE('',*,*,#3288,.F.);
#4050=ORIENTED_EDGE('',*,*,#3287,.F.);
#4051=ORIENTED_EDGE('',*,*,#3286,.T.);
#4052=ORIENTED_EDGE('',*,*,#3289,.F.);
#4053=ORIENTED_EDGE('',*,*,#3290,.T.);
#4054=ORIENTED_EDGE('',*,*,#3291,.F.);
#4055=ORIENTED_EDGE('',*,*,#3290,.F.);
#4056=ORIENTED_EDGE('',*,*,#3292,.F.);
#4057=ORIENTED_EDGE('',*,*,#3293,.F.);
#4058=ORIENTED_EDGE('',*,*,#3294,.F.);
#4059=ORIENTED_EDGE('',*,*,#3295,.F.);
#4060=ORIENTED_EDGE('',*,*,#3288,.T.);
#4061=ORIENTED_EDGE('',*,*,#3296,.F.);
#4062=ORIENTED_EDGE('',*,*,#3297,.F.);
#4063=ORIENTED_EDGE('',*,*,#3298,.F.);
#4064=ORIENTED_EDGE('',*,*,#3299,.F.);
#4065=ORIENTED_EDGE('',*,*,#3289,.T.);
#4066=ORIENTED_EDGE('',*,*,#3293,.T.);
#4067=ORIENTED_EDGE('',*,*,#3300,.T.);
#4068=ORIENTED_EDGE('',*,*,#3301,.T.);
#4069=ORIENTED_EDGE('',*,*,#3302,.F.);
#4070=ORIENTED_EDGE('',*,*,#3303,.T.);
#4071=ORIENTED_EDGE('',*,*,#3304,.T.);
#4072=ORIENTED_EDGE('',*,*,#3299,.T.);
#4073=ORIENTED_EDGE('',*,*,#3305,.T.);
#4074=ORIENTED_EDGE('',*,*,#3294,.T.);
#4075=ORIENTED_EDGE('',*,*,#3305,.F.);
#4076=ORIENTED_EDGE('',*,*,#3298,.T.);
#4077=ORIENTED_EDGE('',*,*,#3306,.F.);
#4078=ORIENTED_EDGE('',*,*,#3296,.T.);
#4079=ORIENTED_EDGE('',*,*,#3304,.F.);
#4080=ORIENTED_EDGE('',*,*,#3307,.F.);
#4081=ORIENTED_EDGE('',*,*,#3308,.F.);
#4082=ORIENTED_EDGE('',*,*,#3309,.F.);
#4083=ORIENTED_EDGE('',*,*,#3310,.F.);
#4084=ORIENTED_EDGE('',*,*,#3301,.F.);
#4085=ORIENTED_EDGE('',*,*,#3311,.F.);
#4086=ORIENTED_EDGE('',*,*,#3292,.T.);
#4087=ORIENTED_EDGE('',*,*,#3312,.F.);
#4088=ORIENTED_EDGE('',*,*,#3311,.T.);
#4089=ORIENTED_EDGE('',*,*,#3300,.F.);
#4090=ORIENTED_EDGE('',*,*,#3313,.F.);
#4091=ORIENTED_EDGE('',*,*,#3307,.T.);
#4092=ORIENTED_EDGE('',*,*,#3303,.F.);
#4093=ORIENTED_EDGE('',*,*,#3314,.F.);
#4094=ORIENTED_EDGE('',*,*,#3291,.T.);
#4095=ORIENTED_EDGE('',*,*,#3295,.T.);
#4096=ORIENTED_EDGE('',*,*,#3306,.T.);
#4097=ORIENTED_EDGE('',*,*,#3297,.T.);
#4098=ORIENTED_EDGE('',*,*,#3308,.T.);
#4099=ORIENTED_EDGE('',*,*,#3313,.T.);
#4100=ORIENTED_EDGE('',*,*,#3315,.F.);
#4101=ORIENTED_EDGE('',*,*,#3309,.T.);
#4102=ORIENTED_EDGE('',*,*,#3312,.T.);
#4103=ORIENTED_EDGE('',*,*,#3316,.F.);
#4104=ORIENTED_EDGE('',*,*,#3317,.T.);
#4105=ORIENTED_EDGE('',*,*,#3318,.F.);
#4106=ORIENTED_EDGE('',*,*,#3317,.F.);
#4107=ORIENTED_EDGE('',*,*,#3316,.T.);
#4108=ORIENTED_EDGE('',*,*,#3319,.F.);
#4109=ORIENTED_EDGE('',*,*,#3320,.T.);
#4110=ORIENTED_EDGE('',*,*,#3321,.F.);
#4111=ORIENTED_EDGE('',*,*,#3320,.F.);
#4112=ORIENTED_EDGE('',*,*,#3322,.F.);
#4113=ORIENTED_EDGE('',*,*,#3323,.F.);
#4114=ORIENTED_EDGE('',*,*,#3324,.F.);
#4115=ORIENTED_EDGE('',*,*,#3325,.F.);
#4116=ORIENTED_EDGE('',*,*,#3318,.T.);
#4117=ORIENTED_EDGE('',*,*,#3326,.F.);
#4118=ORIENTED_EDGE('',*,*,#3327,.F.);
#4119=ORIENTED_EDGE('',*,*,#3328,.F.);
#4120=ORIENTED_EDGE('',*,*,#3329,.F.);
#4121=ORIENTED_EDGE('',*,*,#3319,.T.);
#4122=ORIENTED_EDGE('',*,*,#3323,.T.);
#4123=ORIENTED_EDGE('',*,*,#3330,.T.);
#4124=ORIENTED_EDGE('',*,*,#3331,.T.);
#4125=ORIENTED_EDGE('',*,*,#3332,.F.);
#4126=ORIENTED_EDGE('',*,*,#3333,.T.);
#4127=ORIENTED_EDGE('',*,*,#3334,.T.);
#4128=ORIENTED_EDGE('',*,*,#3329,.T.);
#4129=ORIENTED_EDGE('',*,*,#3335,.T.);
#4130=ORIENTED_EDGE('',*,*,#3324,.T.);
#4131=ORIENTED_EDGE('',*,*,#3335,.F.);
#4132=ORIENTED_EDGE('',*,*,#3328,.T.);
#4133=ORIENTED_EDGE('',*,*,#3336,.F.);
#4134=ORIENTED_EDGE('',*,*,#3326,.T.);
#4135=ORIENTED_EDGE('',*,*,#3334,.F.);
#4136=ORIENTED_EDGE('',*,*,#3337,.F.);
#4137=ORIENTED_EDGE('',*,*,#3338,.F.);
#4138=ORIENTED_EDGE('',*,*,#3339,.F.);
#4139=ORIENTED_EDGE('',*,*,#3340,.F.);
#4140=ORIENTED_EDGE('',*,*,#3331,.F.);
#4141=ORIENTED_EDGE('',*,*,#3341,.F.);
#4142=ORIENTED_EDGE('',*,*,#3322,.T.);
#4143=ORIENTED_EDGE('',*,*,#3342,.F.);
#4144=ORIENTED_EDGE('',*,*,#3341,.T.);
#4145=ORIENTED_EDGE('',*,*,#3330,.F.);
#4146=ORIENTED_EDGE('',*,*,#3343,.F.);
#4147=ORIENTED_EDGE('',*,*,#3337,.T.);
#4148=ORIENTED_EDGE('',*,*,#3333,.F.);
#4149=ORIENTED_EDGE('',*,*,#3344,.F.);
#4150=ORIENTED_EDGE('',*,*,#3321,.T.);
#4151=ORIENTED_EDGE('',*,*,#3325,.T.);
#4152=ORIENTED_EDGE('',*,*,#3336,.T.);
#4153=ORIENTED_EDGE('',*,*,#3327,.T.);
#4154=ORIENTED_EDGE('',*,*,#3338,.T.);
#4155=ORIENTED_EDGE('',*,*,#3343,.T.);
#4156=ORIENTED_EDGE('',*,*,#3345,.F.);
#4157=ORIENTED_EDGE('',*,*,#3339,.T.);
#4158=ORIENTED_EDGE('',*,*,#3342,.T.);
#4159=ORIENTED_EDGE('',*,*,#3346,.T.);
#4160=ORIENTED_EDGE('',*,*,#3347,.T.);
#4161=ORIENTED_EDGE('',*,*,#3348,.F.);
#4162=ORIENTED_EDGE('',*,*,#3349,.F.);
#4163=ORIENTED_EDGE('',*,*,#3350,.T.);
#4164=ORIENTED_EDGE('',*,*,#3349,.T.);
#4165=ORIENTED_EDGE('',*,*,#3351,.F.);
#4166=ORIENTED_EDGE('',*,*,#3352,.F.);
#4167=ORIENTED_EDGE('',*,*,#3344,.T.);
#4168=ORIENTED_EDGE('',*,*,#3332,.T.);
#4169=ORIENTED_EDGE('',*,*,#3340,.T.);
#4170=ORIENTED_EDGE('',*,*,#3345,.T.);
#4171=ORIENTED_EDGE('',*,*,#3314,.T.);
#4172=ORIENTED_EDGE('',*,*,#3302,.T.);
#4173=ORIENTED_EDGE('',*,*,#3310,.T.);
#4174=ORIENTED_EDGE('',*,*,#3315,.T.);
#4175=ORIENTED_EDGE('',*,*,#3285,.T.);
#4176=ORIENTED_EDGE('',*,*,#3279,.T.);
#4177=ORIENTED_EDGE('',*,*,#3276,.T.);
#4178=ORIENTED_EDGE('',*,*,#3273,.T.);
#4179=ORIENTED_EDGE('',*,*,#3270,.T.);
#4180=ORIENTED_EDGE('',*,*,#3353,.T.);
#4181=ORIENTED_EDGE('',*,*,#3352,.T.);
#4182=ORIENTED_EDGE('',*,*,#3354,.F.);
#4183=ORIENTED_EDGE('',*,*,#3355,.F.);
#4184=ORIENTED_EDGE('',*,*,#3356,.T.);
#4185=ORIENTED_EDGE('',*,*,#3355,.T.);
#4186=ORIENTED_EDGE('',*,*,#3357,.F.);
#4187=ORIENTED_EDGE('',*,*,#3347,.F.);
#4188=ORIENTED_EDGE('',*,*,#3280,.T.);
#4189=ORIENTED_EDGE('',*,*,#3277,.T.);
#4190=ORIENTED_EDGE('',*,*,#3274,.T.);
#4191=ORIENTED_EDGE('',*,*,#3271,.T.);
#4192=ORIENTED_EDGE('',*,*,#3268,.T.);
#4193=ORIENTED_EDGE('',*,*,#3357,.T.);
#4194=ORIENTED_EDGE('',*,*,#3354,.T.);
#4195=ORIENTED_EDGE('',*,*,#3351,.T.);
#4196=ORIENTED_EDGE('',*,*,#3348,.T.);
#4197=ORIENTED_EDGE('',*,*,#3356,.F.);
#4198=ORIENTED_EDGE('',*,*,#3346,.F.);
#4199=ORIENTED_EDGE('',*,*,#3350,.F.);
#4200=ORIENTED_EDGE('',*,*,#3353,.F.);
#4201=ORIENTED_EDGE('',*,*,#3358,.F.);
#4202=ORIENTED_EDGE('',*,*,#3359,.T.);
#4203=ORIENTED_EDGE('',*,*,#3360,.F.);
#4204=ORIENTED_EDGE('',*,*,#3359,.F.);
#4205=ORIENTED_EDGE('',*,*,#3361,.T.);
#4206=ORIENTED_EDGE('',*,*,#3362,.T.);
#4207=ORIENTED_EDGE('',*,*,#3363,.F.);
#4208=ORIENTED_EDGE('',*,*,#3364,.F.);
#4209=ORIENTED_EDGE('',*,*,#3365,.T.);
#4210=ORIENTED_EDGE('',*,*,#3364,.T.);
#4211=ORIENTED_EDGE('',*,*,#3366,.F.);
#4212=ORIENTED_EDGE('',*,*,#3367,.F.);
#4213=ORIENTED_EDGE('',*,*,#3368,.T.);
#4214=ORIENTED_EDGE('',*,*,#3367,.T.);
#4215=ORIENTED_EDGE('',*,*,#3369,.F.);
#4216=ORIENTED_EDGE('',*,*,#3370,.F.);
#4217=ORIENTED_EDGE('',*,*,#3371,.T.);
#4218=ORIENTED_EDGE('',*,*,#3370,.T.);
#4219=ORIENTED_EDGE('',*,*,#3372,.F.);
#4220=ORIENTED_EDGE('',*,*,#3373,.F.);
#4221=ORIENTED_EDGE('',*,*,#3374,.T.);
#4222=ORIENTED_EDGE('',*,*,#3373,.T.);
#4223=ORIENTED_EDGE('',*,*,#3375,.F.);
#4224=ORIENTED_EDGE('',*,*,#3376,.F.);
#4225=ORIENTED_EDGE('',*,*,#3377,.T.);
#4226=ORIENTED_EDGE('',*,*,#3376,.T.);
#4227=ORIENTED_EDGE('',*,*,#3378,.F.);
#4228=ORIENTED_EDGE('',*,*,#3362,.F.);
#4229=ORIENTED_EDGE('',*,*,#3378,.T.);
#4230=ORIENTED_EDGE('',*,*,#3375,.T.);
#4231=ORIENTED_EDGE('',*,*,#3372,.T.);
#4232=ORIENTED_EDGE('',*,*,#3369,.T.);
#4233=ORIENTED_EDGE('',*,*,#3366,.T.);
#4234=ORIENTED_EDGE('',*,*,#3363,.T.);
#4235=ORIENTED_EDGE('',*,*,#3360,.T.);
#4236=ORIENTED_EDGE('',*,*,#3377,.F.);
#4237=ORIENTED_EDGE('',*,*,#3361,.F.);
#4238=ORIENTED_EDGE('',*,*,#3365,.F.);
#4239=ORIENTED_EDGE('',*,*,#3368,.F.);
#4240=ORIENTED_EDGE('',*,*,#3371,.F.);
#4241=ORIENTED_EDGE('',*,*,#3374,.F.);
#4242=ORIENTED_EDGE('',*,*,#3358,.T.);
#4243=ORIENTED_EDGE('',*,*,#3379,.F.);
#4244=ORIENTED_EDGE('',*,*,#3380,.T.);
#4245=ORIENTED_EDGE('',*,*,#3381,.F.);
#4246=ORIENTED_EDGE('',*,*,#3382,.T.);
#4247=ORIENTED_EDGE('',*,*,#3379,.T.);
#4248=ORIENTED_EDGE('',*,*,#3382,.F.);
#4249=ORIENTED_EDGE('',*,*,#3381,.T.);
#4250=ORIENTED_EDGE('',*,*,#3383,.F.);
#4251=ORIENTED_EDGE('',*,*,#3384,.F.);
#4252=ORIENTED_EDGE('',*,*,#3385,.T.);
#4253=ORIENTED_EDGE('',*,*,#3383,.T.);
#4254=ORIENTED_EDGE('',*,*,#3385,.F.);
#4255=ORIENTED_EDGE('',*,*,#3386,.F.);
#4256=ORIENTED_EDGE('',*,*,#3387,.T.);
#4257=ORIENTED_EDGE('',*,*,#3384,.T.);
#4258=ORIENTED_EDGE('',*,*,#3387,.F.);
#4259=ORIENTED_EDGE('',*,*,#3386,.T.);
#4260=ORIENTED_EDGE('',*,*,#3388,.F.);
#4261=ORIENTED_EDGE('',*,*,#3389,.F.);
#4262=ORIENTED_EDGE('',*,*,#3390,.T.);
#4263=ORIENTED_EDGE('',*,*,#3388,.T.);
#4264=ORIENTED_EDGE('',*,*,#3390,.F.);
#4265=ORIENTED_EDGE('',*,*,#3391,.F.);
#4266=ORIENTED_EDGE('',*,*,#3392,.T.);
#4267=ORIENTED_EDGE('',*,*,#3389,.T.);
#4268=ORIENTED_EDGE('',*,*,#3392,.F.);
#4269=ORIENTED_EDGE('',*,*,#3391,.T.);
#4270=ORIENTED_EDGE('',*,*,#3393,.F.);
#4271=ORIENTED_EDGE('',*,*,#3394,.F.);
#4272=ORIENTED_EDGE('',*,*,#3395,.T.);
#4273=ORIENTED_EDGE('',*,*,#3393,.T.);
#4274=ORIENTED_EDGE('',*,*,#3395,.F.);
#4275=ORIENTED_EDGE('',*,*,#3396,.T.);
#4276=ORIENTED_EDGE('',*,*,#3397,.T.);
#4277=ORIENTED_EDGE('',*,*,#3380,.F.);
#4278=ORIENTED_EDGE('',*,*,#3397,.F.);
#4279=ORIENTED_EDGE('',*,*,#3398,.T.);
#4280=ORIENTED_EDGE('',*,*,#3399,.T.);
#4281=ORIENTED_EDGE('',*,*,#3400,.T.);
#4282=ORIENTED_EDGE('',*,*,#3401,.T.);
#4283=ORIENTED_EDGE('',*,*,#3402,.T.);
#4284=ORIENTED_EDGE('',*,*,#3403,.T.);
#4285=ORIENTED_EDGE('',*,*,#3404,.T.);
#4286=ORIENTED_EDGE('',*,*,#3399,.F.);
#4287=ORIENTED_EDGE('',*,*,#3405,.T.);
#4288=ORIENTED_EDGE('',*,*,#3406,.F.);
#4289=ORIENTED_EDGE('',*,*,#3407,.F.);
#4290=ORIENTED_EDGE('',*,*,#3400,.F.);
#4291=ORIENTED_EDGE('',*,*,#3407,.T.);
#4292=ORIENTED_EDGE('',*,*,#3408,.F.);
#4293=ORIENTED_EDGE('',*,*,#3409,.F.);
#4294=ORIENTED_EDGE('',*,*,#3401,.F.);
#4295=ORIENTED_EDGE('',*,*,#3409,.T.);
#4296=ORIENTED_EDGE('',*,*,#3410,.F.);
#4297=ORIENTED_EDGE('',*,*,#3411,.F.);
#4298=ORIENTED_EDGE('',*,*,#3402,.F.);
#4299=ORIENTED_EDGE('',*,*,#3411,.T.);
#4300=ORIENTED_EDGE('',*,*,#3412,.F.);
#4301=ORIENTED_EDGE('',*,*,#3413,.F.);
#4302=ORIENTED_EDGE('',*,*,#3403,.F.);
#4303=ORIENTED_EDGE('',*,*,#3413,.T.);
#4304=ORIENTED_EDGE('',*,*,#3414,.F.);
#4305=ORIENTED_EDGE('',*,*,#3415,.F.);
#4306=ORIENTED_EDGE('',*,*,#3398,.F.);
#4307=ORIENTED_EDGE('',*,*,#3415,.T.);
#4308=ORIENTED_EDGE('',*,*,#3416,.F.);
#4309=ORIENTED_EDGE('',*,*,#3405,.F.);
#4310=ORIENTED_EDGE('',*,*,#3416,.T.);
#4311=ORIENTED_EDGE('',*,*,#3414,.T.);
#4312=ORIENTED_EDGE('',*,*,#3412,.T.);
#4313=ORIENTED_EDGE('',*,*,#3410,.T.);
#4314=ORIENTED_EDGE('',*,*,#3408,.T.);
#4315=ORIENTED_EDGE('',*,*,#3406,.T.);
#4316=ORIENTED_EDGE('',*,*,#3394,.T.);
#4317=ORIENTED_EDGE('',*,*,#3404,.F.);
#4318=ORIENTED_EDGE('',*,*,#3417,.T.);
#4319=ORIENTED_EDGE('',*,*,#3418,.T.);
#4320=ORIENTED_EDGE('',*,*,#3417,.F.);
#4321=ORIENTED_EDGE('',*,*,#3418,.F.);
#4322=ORIENTED_EDGE('',*,*,#3396,.F.);
#4323=ORIENTED_EDGE('',*,*,#3419,.F.);
#4324=ORIENTED_EDGE('',*,*,#3420,.T.);
#4325=ORIENTED_EDGE('',*,*,#3421,.F.);
#4326=ORIENTED_EDGE('',*,*,#3420,.F.);
#4327=ORIENTED_EDGE('',*,*,#3419,.T.);
#4328=ORIENTED_EDGE('',*,*,#3422,.F.);
#4329=ORIENTED_EDGE('',*,*,#3423,.T.);
#4330=ORIENTED_EDGE('',*,*,#3424,.F.);
#4331=ORIENTED_EDGE('',*,*,#3423,.F.);
#4332=ORIENTED_EDGE('',*,*,#3422,.T.);
#4333=ORIENTED_EDGE('',*,*,#3425,.F.);
#4334=ORIENTED_EDGE('',*,*,#3426,.T.);
#4335=ORIENTED_EDGE('',*,*,#3427,.F.);
#4336=ORIENTED_EDGE('',*,*,#3426,.F.);
#4337=ORIENTED_EDGE('',*,*,#3428,.F.);
#4338=ORIENTED_EDGE('',*,*,#3429,.T.);
#4339=ORIENTED_EDGE('',*,*,#3430,.F.);
#4340=ORIENTED_EDGE('',*,*,#3429,.F.);
#4341=ORIENTED_EDGE('',*,*,#3431,.F.);
#4342=ORIENTED_EDGE('',*,*,#3432,.T.);
#4343=ORIENTED_EDGE('',*,*,#3433,.F.);
#4344=ORIENTED_EDGE('',*,*,#3432,.F.);
#4345=ORIENTED_EDGE('',*,*,#3434,.F.);
#4346=ORIENTED_EDGE('',*,*,#3435,.T.);
#4347=ORIENTED_EDGE('',*,*,#3436,.F.);
#4348=ORIENTED_EDGE('',*,*,#3435,.F.);
#4349=ORIENTED_EDGE('',*,*,#3437,.F.);
#4350=ORIENTED_EDGE('',*,*,#3438,.F.);
#4351=ORIENTED_EDGE('',*,*,#3439,.F.);
#4352=ORIENTED_EDGE('',*,*,#3440,.F.);
#4353=ORIENTED_EDGE('',*,*,#3441,.F.);
#4354=ORIENTED_EDGE('',*,*,#3442,.F.);
#4355=ORIENTED_EDGE('',*,*,#3443,.F.);
#4356=ORIENTED_EDGE('',*,*,#3438,.T.);
#4357=ORIENTED_EDGE('',*,*,#3440,.T.);
#4358=ORIENTED_EDGE('',*,*,#3444,.T.);
#4359=ORIENTED_EDGE('',*,*,#3445,.T.);
#4360=ORIENTED_EDGE('',*,*,#3446,.T.);
#4361=ORIENTED_EDGE('',*,*,#3447,.T.);
#4362=ORIENTED_EDGE('',*,*,#3448,.T.);
#4363=ORIENTED_EDGE('',*,*,#3421,.T.);
#4364=ORIENTED_EDGE('',*,*,#3424,.T.);
#4365=ORIENTED_EDGE('',*,*,#3449,.F.);
#4366=ORIENTED_EDGE('',*,*,#3450,.T.);
#4367=ORIENTED_EDGE('',*,*,#3451,.F.);
#4368=ORIENTED_EDGE('',*,*,#3450,.F.);
#4369=ORIENTED_EDGE('',*,*,#3452,.F.);
#4370=ORIENTED_EDGE('',*,*,#3453,.T.);
#4371=ORIENTED_EDGE('',*,*,#3454,.T.);
#4372=ORIENTED_EDGE('',*,*,#3453,.F.);
#4373=ORIENTED_EDGE('',*,*,#3454,.F.);
#4374=ORIENTED_EDGE('',*,*,#3455,.F.);
#4375=ORIENTED_EDGE('',*,*,#3452,.T.);
#4376=ORIENTED_EDGE('',*,*,#3451,.T.);
#4377=ORIENTED_EDGE('',*,*,#3442,.T.);
#4378=ORIENTED_EDGE('',*,*,#3456,.F.);
#4379=ORIENTED_EDGE('',*,*,#3455,.T.);
#4380=ORIENTED_EDGE('',*,*,#3437,.T.);
#4381=ORIENTED_EDGE('',*,*,#3448,.F.);
#4382=ORIENTED_EDGE('',*,*,#3457,.F.);
#4383=ORIENTED_EDGE('',*,*,#3458,.T.);
#4384=ORIENTED_EDGE('',*,*,#3459,.T.);
#4385=ORIENTED_EDGE('',*,*,#3444,.F.);
#4386=ORIENTED_EDGE('',*,*,#3439,.T.);
#4387=ORIENTED_EDGE('',*,*,#3443,.T.);
#4388=ORIENTED_EDGE('',*,*,#3456,.T.);
#4389=ORIENTED_EDGE('',*,*,#3441,.T.);
#4390=ORIENTED_EDGE('',*,*,#3427,.T.);
#4391=ORIENTED_EDGE('',*,*,#3430,.T.);
#4392=ORIENTED_EDGE('',*,*,#3433,.T.);
#4393=ORIENTED_EDGE('',*,*,#3436,.T.);
#4394=ORIENTED_EDGE('',*,*,#3460,.T.);
#4395=ORIENTED_EDGE('',*,*,#3457,.T.);
#4396=ORIENTED_EDGE('',*,*,#3447,.F.);
#4397=ORIENTED_EDGE('',*,*,#3461,.F.);
#4398=ORIENTED_EDGE('',*,*,#3462,.T.);
#4399=ORIENTED_EDGE('',*,*,#3461,.T.);
#4400=ORIENTED_EDGE('',*,*,#3446,.F.);
#4401=ORIENTED_EDGE('',*,*,#3463,.F.);
#4402=ORIENTED_EDGE('',*,*,#3449,.T.);
#4403=ORIENTED_EDGE('',*,*,#3434,.T.);
#4404=ORIENTED_EDGE('',*,*,#3431,.T.);
#4405=ORIENTED_EDGE('',*,*,#3428,.T.);
#4406=ORIENTED_EDGE('',*,*,#3425,.T.);
#4407=ORIENTED_EDGE('',*,*,#3464,.T.);
#4408=ORIENTED_EDGE('',*,*,#3463,.T.);
#4409=ORIENTED_EDGE('',*,*,#3445,.F.);
#4410=ORIENTED_EDGE('',*,*,#3459,.F.);
#4411=ORIENTED_EDGE('',*,*,#3464,.F.);
#4412=ORIENTED_EDGE('',*,*,#3458,.F.);
#4413=ORIENTED_EDGE('',*,*,#3460,.F.);
#4414=ORIENTED_EDGE('',*,*,#3462,.F.);
#4415=ORIENTED_EDGE('',*,*,#3465,.F.);
#4416=ORIENTED_EDGE('',*,*,#3466,.T.);
#4417=ORIENTED_EDGE('',*,*,#3467,.F.);
#4418=ORIENTED_EDGE('',*,*,#3466,.F.);
#4419=ORIENTED_EDGE('',*,*,#3465,.T.);
#4420=ORIENTED_EDGE('',*,*,#3468,.F.);
#4421=ORIENTED_EDGE('',*,*,#3469,.T.);
#4422=ORIENTED_EDGE('',*,*,#3470,.F.);
#4423=ORIENTED_EDGE('',*,*,#3469,.F.);
#4424=ORIENTED_EDGE('',*,*,#3468,.T.);
#4425=ORIENTED_EDGE('',*,*,#3471,.F.);
#4426=ORIENTED_EDGE('',*,*,#3472,.T.);
#4427=ORIENTED_EDGE('',*,*,#3473,.F.);
#4428=ORIENTED_EDGE('',*,*,#3472,.F.);
#4429=ORIENTED_EDGE('',*,*,#3474,.F.);
#4430=ORIENTED_EDGE('',*,*,#3475,.T.);
#4431=ORIENTED_EDGE('',*,*,#3476,.F.);
#4432=ORIENTED_EDGE('',*,*,#3475,.F.);
#4433=ORIENTED_EDGE('',*,*,#3477,.F.);
#4434=ORIENTED_EDGE('',*,*,#3478,.T.);
#4435=ORIENTED_EDGE('',*,*,#3479,.F.);
#4436=ORIENTED_EDGE('',*,*,#3478,.F.);
#4437=ORIENTED_EDGE('',*,*,#3480,.F.);
#4438=ORIENTED_EDGE('',*,*,#3481,.T.);
#4439=ORIENTED_EDGE('',*,*,#3482,.F.);
#4440=ORIENTED_EDGE('',*,*,#3481,.F.);
#4441=ORIENTED_EDGE('',*,*,#3483,.F.);
#4442=ORIENTED_EDGE('',*,*,#3484,.F.);
#4443=ORIENTED_EDGE('',*,*,#3485,.F.);
#4444=ORIENTED_EDGE('',*,*,#3486,.F.);
#4445=ORIENTED_EDGE('',*,*,#3487,.F.);
#4446=ORIENTED_EDGE('',*,*,#3488,.F.);
#4447=ORIENTED_EDGE('',*,*,#3489,.F.);
#4448=ORIENTED_EDGE('',*,*,#3484,.T.);
#4449=ORIENTED_EDGE('',*,*,#3486,.T.);
#4450=ORIENTED_EDGE('',*,*,#3490,.T.);
#4451=ORIENTED_EDGE('',*,*,#3491,.T.);
#4452=ORIENTED_EDGE('',*,*,#3492,.T.);
#4453=ORIENTED_EDGE('',*,*,#3493,.T.);
#4454=ORIENTED_EDGE('',*,*,#3494,.T.);
#4455=ORIENTED_EDGE('',*,*,#3467,.T.);
#4456=ORIENTED_EDGE('',*,*,#3470,.T.);
#4457=ORIENTED_EDGE('',*,*,#3495,.F.);
#4458=ORIENTED_EDGE('',*,*,#3496,.T.);
#4459=ORIENTED_EDGE('',*,*,#3497,.F.);
#4460=ORIENTED_EDGE('',*,*,#3496,.F.);
#4461=ORIENTED_EDGE('',*,*,#3498,.F.);
#4462=ORIENTED_EDGE('',*,*,#3499,.T.);
#4463=ORIENTED_EDGE('',*,*,#3500,.T.);
#4464=ORIENTED_EDGE('',*,*,#3499,.F.);
#4465=ORIENTED_EDGE('',*,*,#3500,.F.);
#4466=ORIENTED_EDGE('',*,*,#3495,.T.);
#4467=ORIENTED_EDGE('',*,*,#3498,.T.);
#4468=ORIENTED_EDGE('',*,*,#3501,.F.);
#4469=ORIENTED_EDGE('',*,*,#3488,.T.);
#4470=ORIENTED_EDGE('',*,*,#3502,.F.);
#4471=ORIENTED_EDGE('',*,*,#3501,.T.);
#4472=ORIENTED_EDGE('',*,*,#3503,.T.);
#4473=ORIENTED_EDGE('',*,*,#3504,.T.);
#4474=ORIENTED_EDGE('',*,*,#3492,.F.);
#4475=ORIENTED_EDGE('',*,*,#3505,.F.);
#4476=ORIENTED_EDGE('',*,*,#3497,.T.);
#4477=ORIENTED_EDGE('',*,*,#3482,.T.);
#4478=ORIENTED_EDGE('',*,*,#3479,.T.);
#4479=ORIENTED_EDGE('',*,*,#3476,.T.);
#4480=ORIENTED_EDGE('',*,*,#3473,.T.);
#4481=ORIENTED_EDGE('',*,*,#3506,.T.);
#4482=ORIENTED_EDGE('',*,*,#3505,.T.);
#4483=ORIENTED_EDGE('',*,*,#3491,.F.);
#4484=ORIENTED_EDGE('',*,*,#3507,.F.);
#4485=ORIENTED_EDGE('',*,*,#3483,.T.);
#4486=ORIENTED_EDGE('',*,*,#3494,.F.);
#4487=ORIENTED_EDGE('',*,*,#3508,.F.);
#4488=ORIENTED_EDGE('',*,*,#3509,.T.);
#4489=ORIENTED_EDGE('',*,*,#3507,.T.);
#4490=ORIENTED_EDGE('',*,*,#3490,.F.);
#4491=ORIENTED_EDGE('',*,*,#3485,.T.);
#4492=ORIENTED_EDGE('',*,*,#3489,.T.);
#4493=ORIENTED_EDGE('',*,*,#3502,.T.);
#4494=ORIENTED_EDGE('',*,*,#3487,.T.);
#4495=ORIENTED_EDGE('',*,*,#3471,.T.);
#4496=ORIENTED_EDGE('',*,*,#3474,.T.);
#4497=ORIENTED_EDGE('',*,*,#3477,.T.);
#4498=ORIENTED_EDGE('',*,*,#3480,.T.);
#4499=ORIENTED_EDGE('',*,*,#3510,.T.);
#4500=ORIENTED_EDGE('',*,*,#3508,.T.);
#4501=ORIENTED_EDGE('',*,*,#3493,.F.);
#4502=ORIENTED_EDGE('',*,*,#3504,.F.);
#4503=ORIENTED_EDGE('',*,*,#3510,.F.);
#4504=ORIENTED_EDGE('',*,*,#3503,.F.);
#4505=ORIENTED_EDGE('',*,*,#3506,.F.);
#4506=ORIENTED_EDGE('',*,*,#3509,.F.);
#4507=ORIENTED_EDGE('',*,*,#3511,.F.);
#4508=ORIENTED_EDGE('',*,*,#3512,.T.);
#4509=ORIENTED_EDGE('',*,*,#3513,.F.);
#4510=ORIENTED_EDGE('',*,*,#3512,.F.);
#4511=ORIENTED_EDGE('',*,*,#3514,.F.);
#4512=ORIENTED_EDGE('',*,*,#3515,.T.);
#4513=ORIENTED_EDGE('',*,*,#3516,.F.);
#4514=ORIENTED_EDGE('',*,*,#3515,.F.);
#4515=ORIENTED_EDGE('',*,*,#3517,.F.);
#4516=ORIENTED_EDGE('',*,*,#3518,.T.);
#4517=ORIENTED_EDGE('',*,*,#3519,.F.);
#4518=ORIENTED_EDGE('',*,*,#3518,.F.);
#4519=ORIENTED_EDGE('',*,*,#3520,.F.);
#4520=ORIENTED_EDGE('',*,*,#3521,.T.);
#4521=ORIENTED_EDGE('',*,*,#3522,.F.);
#4522=ORIENTED_EDGE('',*,*,#3521,.F.);
#4523=ORIENTED_EDGE('',*,*,#3523,.F.);
#4524=ORIENTED_EDGE('',*,*,#3524,.T.);
#4525=ORIENTED_EDGE('',*,*,#3525,.F.);
#4526=ORIENTED_EDGE('',*,*,#3526,.F.);
#4527=ORIENTED_EDGE('',*,*,#3527,.F.);
#4528=ORIENTED_EDGE('',*,*,#3528,.T.);
#4529=ORIENTED_EDGE('',*,*,#3529,.F.);
#4530=ORIENTED_EDGE('',*,*,#3530,.F.);
#4531=ORIENTED_EDGE('',*,*,#3531,.F.);
#4532=ORIENTED_EDGE('',*,*,#3532,.F.);
#4533=ORIENTED_EDGE('',*,*,#3533,.F.);
#4534=ORIENTED_EDGE('',*,*,#3524,.F.);
#4535=ORIENTED_EDGE('',*,*,#3534,.F.);
#4536=ORIENTED_EDGE('',*,*,#3535,.F.);
#4537=ORIENTED_EDGE('',*,*,#3536,.F.);
#4538=ORIENTED_EDGE('',*,*,#3528,.F.);
#4539=ORIENTED_EDGE('',*,*,#3525,.T.);
#4540=ORIENTED_EDGE('',*,*,#3533,.T.);
#4541=ORIENTED_EDGE('',*,*,#3537,.T.);
#4542=ORIENTED_EDGE('',*,*,#3529,.T.);
#4543=ORIENTED_EDGE('',*,*,#3536,.T.);
#4544=ORIENTED_EDGE('',*,*,#3538,.T.);
#4545=ORIENTED_EDGE('',*,*,#3539,.T.);
#4546=ORIENTED_EDGE('',*,*,#3540,.T.);
#4547=ORIENTED_EDGE('',*,*,#3541,.T.);
#4548=ORIENTED_EDGE('',*,*,#3542,.T.);
#4549=ORIENTED_EDGE('',*,*,#3513,.T.);
#4550=ORIENTED_EDGE('',*,*,#3516,.T.);
#4551=ORIENTED_EDGE('',*,*,#3519,.T.);
#4552=ORIENTED_EDGE('',*,*,#3522,.T.);
#4553=ORIENTED_EDGE('',*,*,#3535,.T.);
#4554=ORIENTED_EDGE('',*,*,#3543,.F.);
#4555=ORIENTED_EDGE('',*,*,#3544,.T.);
#4556=ORIENTED_EDGE('',*,*,#3538,.F.);
#4557=ORIENTED_EDGE('',*,*,#3526,.T.);
#4558=ORIENTED_EDGE('',*,*,#3542,.F.);
#4559=ORIENTED_EDGE('',*,*,#3545,.F.);
#4560=ORIENTED_EDGE('',*,*,#3546,.F.);
#4561=ORIENTED_EDGE('',*,*,#3532,.T.);
#4562=ORIENTED_EDGE('',*,*,#3547,.F.);
#4563=ORIENTED_EDGE('',*,*,#3530,.T.);
#4564=ORIENTED_EDGE('',*,*,#3537,.F.);
#4565=ORIENTED_EDGE('',*,*,#3548,.F.);
#4566=ORIENTED_EDGE('',*,*,#3545,.T.);
#4567=ORIENTED_EDGE('',*,*,#3541,.F.);
#4568=ORIENTED_EDGE('',*,*,#3549,.F.);
#4569=ORIENTED_EDGE('',*,*,#3550,.F.);
#4570=ORIENTED_EDGE('',*,*,#3549,.T.);
#4571=ORIENTED_EDGE('',*,*,#3540,.F.);
#4572=ORIENTED_EDGE('',*,*,#3551,.F.);
#4573=ORIENTED_EDGE('',*,*,#3552,.F.);
#4574=ORIENTED_EDGE('',*,*,#3551,.T.);
#4575=ORIENTED_EDGE('',*,*,#3539,.F.);
#4576=ORIENTED_EDGE('',*,*,#3544,.F.);
#4577=ORIENTED_EDGE('',*,*,#3523,.T.);
#4578=ORIENTED_EDGE('',*,*,#3546,.T.);
#4579=ORIENTED_EDGE('',*,*,#3548,.T.);
#4580=ORIENTED_EDGE('',*,*,#3550,.T.);
#4581=ORIENTED_EDGE('',*,*,#3552,.T.);
#4582=ORIENTED_EDGE('',*,*,#3543,.T.);
#4583=ORIENTED_EDGE('',*,*,#3534,.T.);
#4584=ORIENTED_EDGE('',*,*,#3527,.T.);
#4585=ORIENTED_EDGE('',*,*,#3547,.T.);
#4586=ORIENTED_EDGE('',*,*,#3531,.T.);
#4587=ORIENTED_EDGE('',*,*,#3511,.T.);
#4588=ORIENTED_EDGE('',*,*,#3514,.T.);
#4589=ORIENTED_EDGE('',*,*,#3517,.T.);
#4590=ORIENTED_EDGE('',*,*,#3520,.T.);
#4591=ORIENTED_EDGE('',*,*,#3553,.F.);
#4592=ORIENTED_EDGE('',*,*,#3554,.T.);
#4593=ORIENTED_EDGE('',*,*,#3555,.F.);
#4594=ORIENTED_EDGE('',*,*,#3556,.T.);
#4595=ORIENTED_EDGE('',*,*,#3553,.T.);
#4596=ORIENTED_EDGE('',*,*,#3556,.F.);
#4597=ORIENTED_EDGE('',*,*,#3555,.T.);
#4598=ORIENTED_EDGE('',*,*,#3557,.T.);
#4599=ORIENTED_EDGE('',*,*,#3557,.F.);
#4600=ORIENTED_EDGE('',*,*,#3558,.T.);
#4601=ORIENTED_EDGE('',*,*,#3559,.T.);
#4602=ORIENTED_EDGE('',*,*,#3558,.F.);
#4603=ORIENTED_EDGE('',*,*,#3554,.F.);
#4604=ORIENTED_EDGE('',*,*,#3560,.T.);
#4605=ORIENTED_EDGE('',*,*,#3561,.T.);
#4606=ORIENTED_EDGE('',*,*,#3560,.F.);
#4607=ORIENTED_EDGE('',*,*,#3561,.F.);
#4608=ORIENTED_EDGE('',*,*,#3559,.F.);
#4609=ORIENTED_EDGE('',*,*,#3562,.F.);
#4610=ORIENTED_EDGE('',*,*,#3563,.T.);
#4611=ORIENTED_EDGE('',*,*,#3562,.T.);
#4612=ORIENTED_EDGE('',*,*,#3563,.F.);
#4613=ORIENTED_EDGE('',*,*,#3564,.F.);
#4614=ORIENTED_EDGE('',*,*,#3565,.T.);
#4615=ORIENTED_EDGE('',*,*,#3566,.T.);
#4616=ORIENTED_EDGE('',*,*,#3565,.F.);
#4617=ORIENTED_EDGE('',*,*,#3566,.F.);
#4618=ORIENTED_EDGE('',*,*,#3567,.F.);
#4619=ORIENTED_EDGE('',*,*,#3568,.F.);
#4620=ORIENTED_EDGE('',*,*,#3569,.T.);
#4621=ORIENTED_EDGE('',*,*,#3567,.T.);
#4622=ORIENTED_EDGE('',*,*,#3569,.F.);
#4623=ORIENTED_EDGE('',*,*,#3570,.F.);
#4624=ORIENTED_EDGE('',*,*,#3571,.T.);
#4625=ORIENTED_EDGE('',*,*,#3572,.T.);
#4626=ORIENTED_EDGE('',*,*,#3571,.F.);
#4627=ORIENTED_EDGE('',*,*,#3570,.T.);
#4628=ORIENTED_EDGE('',*,*,#3568,.T.);
#4629=ORIENTED_EDGE('',*,*,#3572,.F.);
#4630=ORIENTED_EDGE('',*,*,#3564,.T.);
#4631=ORIENTED_EDGE('',*,*,#3573,.F.);
#4632=ORIENTED_EDGE('',*,*,#3574,.T.);
#4633=ORIENTED_EDGE('',*,*,#3575,.F.);
#4634=ORIENTED_EDGE('',*,*,#3574,.F.);
#4635=ORIENTED_EDGE('',*,*,#3573,.T.);
#4636=ORIENTED_EDGE('',*,*,#3576,.F.);
#4637=ORIENTED_EDGE('',*,*,#3577,.T.);
#4638=ORIENTED_EDGE('',*,*,#3578,.F.);
#4639=ORIENTED_EDGE('',*,*,#3577,.F.);
#4640=ORIENTED_EDGE('',*,*,#3576,.T.);
#4641=ORIENTED_EDGE('',*,*,#3579,.F.);
#4642=ORIENTED_EDGE('',*,*,#3580,.T.);
#4643=ORIENTED_EDGE('',*,*,#3581,.F.);
#4644=ORIENTED_EDGE('',*,*,#3580,.F.);
#4645=ORIENTED_EDGE('',*,*,#3582,.F.);
#4646=ORIENTED_EDGE('',*,*,#3583,.T.);
#4647=ORIENTED_EDGE('',*,*,#3584,.F.);
#4648=ORIENTED_EDGE('',*,*,#3583,.F.);
#4649=ORIENTED_EDGE('',*,*,#3585,.F.);
#4650=ORIENTED_EDGE('',*,*,#3586,.T.);
#4651=ORIENTED_EDGE('',*,*,#3587,.F.);
#4652=ORIENTED_EDGE('',*,*,#3586,.F.);
#4653=ORIENTED_EDGE('',*,*,#3588,.F.);
#4654=ORIENTED_EDGE('',*,*,#3589,.T.);
#4655=ORIENTED_EDGE('',*,*,#3590,.F.);
#4656=ORIENTED_EDGE('',*,*,#3589,.F.);
#4657=ORIENTED_EDGE('',*,*,#3591,.F.);
#4658=ORIENTED_EDGE('',*,*,#3592,.T.);
#4659=ORIENTED_EDGE('',*,*,#3593,.F.);
#4660=ORIENTED_EDGE('',*,*,#3592,.F.);
#4661=ORIENTED_EDGE('',*,*,#3594,.T.);
#4662=ORIENTED_EDGE('',*,*,#3595,.T.);
#4663=ORIENTED_EDGE('',*,*,#3596,.F.);
#4664=ORIENTED_EDGE('',*,*,#3597,.F.);
#4665=ORIENTED_EDGE('',*,*,#3598,.T.);
#4666=ORIENTED_EDGE('',*,*,#3597,.T.);
#4667=ORIENTED_EDGE('',*,*,#3599,.F.);
#4668=ORIENTED_EDGE('',*,*,#3600,.F.);
#4669=ORIENTED_EDGE('',*,*,#3601,.T.);
#4670=ORIENTED_EDGE('',*,*,#3600,.T.);
#4671=ORIENTED_EDGE('',*,*,#3602,.F.);
#4672=ORIENTED_EDGE('',*,*,#3603,.F.);
#4673=ORIENTED_EDGE('',*,*,#3604,.T.);
#4674=ORIENTED_EDGE('',*,*,#3603,.T.);
#4675=ORIENTED_EDGE('',*,*,#3605,.F.);
#4676=ORIENTED_EDGE('',*,*,#3595,.F.);
#4677=ORIENTED_EDGE('',*,*,#3605,.T.);
#4678=ORIENTED_EDGE('',*,*,#3602,.T.);
#4679=ORIENTED_EDGE('',*,*,#3599,.T.);
#4680=ORIENTED_EDGE('',*,*,#3596,.T.);
#4681=ORIENTED_EDGE('',*,*,#3575,.T.);
#4682=ORIENTED_EDGE('',*,*,#3578,.T.);
#4683=ORIENTED_EDGE('',*,*,#3593,.T.);
#4684=ORIENTED_EDGE('',*,*,#3590,.T.);
#4685=ORIENTED_EDGE('',*,*,#3587,.T.);
#4686=ORIENTED_EDGE('',*,*,#3584,.T.);
#4687=ORIENTED_EDGE('',*,*,#3581,.T.);
#4688=ORIENTED_EDGE('',*,*,#3604,.F.);
#4689=ORIENTED_EDGE('',*,*,#3594,.F.);
#4690=ORIENTED_EDGE('',*,*,#3598,.F.);
#4691=ORIENTED_EDGE('',*,*,#3601,.F.);
#4692=ORIENTED_EDGE('',*,*,#3591,.T.);
#4693=ORIENTED_EDGE('',*,*,#3588,.T.);
#4694=ORIENTED_EDGE('',*,*,#3585,.T.);
#4695=ORIENTED_EDGE('',*,*,#3582,.T.);
#4696=ORIENTED_EDGE('',*,*,#3579,.T.);
#4697=ORIENTED_EDGE('',*,*,#3606,.F.);
#4698=ORIENTED_EDGE('',*,*,#3607,.F.);
#4699=ORIENTED_EDGE('',*,*,#3607,.T.);
#4700=ORIENTED_EDGE('',*,*,#3608,.T.);
#4701=ORIENTED_EDGE('',*,*,#3609,.T.);
#4702=ORIENTED_EDGE('',*,*,#3608,.F.);
#4703=ORIENTED_EDGE('',*,*,#3610,.F.);
#4704=ORIENTED_EDGE('',*,*,#3611,.T.);
#4705=ORIENTED_EDGE('',*,*,#3612,.T.);
#4706=ORIENTED_EDGE('',*,*,#3611,.F.);
#4707=ORIENTED_EDGE('',*,*,#3610,.T.);
#4708=ORIENTED_EDGE('',*,*,#3606,.T.);
#4709=ORIENTED_EDGE('',*,*,#3612,.F.);
#4710=ORIENTED_EDGE('',*,*,#3609,.F.);
#4711=ORIENTED_EDGE('',*,*,#3613,.T.);
#4712=ORIENTED_EDGE('',*,*,#3614,.T.);
#4713=ORIENTED_EDGE('',*,*,#3615,.T.);
#4714=ORIENTED_EDGE('',*,*,#3616,.F.);
#4715=ORIENTED_EDGE('',*,*,#3617,.T.);
#4716=ORIENTED_EDGE('',*,*,#3618,.T.);
#4717=ORIENTED_EDGE('',*,*,#3619,.T.);
#4718=ORIENTED_EDGE('',*,*,#3614,.F.);
#4719=ORIENTED_EDGE('',*,*,#3620,.T.);
#4720=ORIENTED_EDGE('',*,*,#3621,.T.);
#4721=ORIENTED_EDGE('',*,*,#3622,.T.);
#4722=ORIENTED_EDGE('',*,*,#3618,.F.);
#4723=ORIENTED_EDGE('',*,*,#3623,.T.);
#4724=ORIENTED_EDGE('',*,*,#3624,.T.);
#4725=ORIENTED_EDGE('',*,*,#3625,.T.);
#4726=ORIENTED_EDGE('',*,*,#3621,.F.);
#4727=ORIENTED_EDGE('',*,*,#3626,.T.);
#4728=ORIENTED_EDGE('',*,*,#3627,.T.);
#4729=ORIENTED_EDGE('',*,*,#3628,.T.);
#4730=ORIENTED_EDGE('',*,*,#3624,.F.);
#4731=ORIENTED_EDGE('',*,*,#3629,.T.);
#4732=ORIENTED_EDGE('',*,*,#3616,.T.);
#4733=ORIENTED_EDGE('',*,*,#3630,.T.);
#4734=ORIENTED_EDGE('',*,*,#3627,.F.);
#4735=ORIENTED_EDGE('',*,*,#3629,.F.);
#4736=ORIENTED_EDGE('',*,*,#3626,.F.);
#4737=ORIENTED_EDGE('',*,*,#3623,.F.);
#4738=ORIENTED_EDGE('',*,*,#3620,.F.);
#4739=ORIENTED_EDGE('',*,*,#3617,.F.);
#4740=ORIENTED_EDGE('',*,*,#3613,.F.);
#4741=ORIENTED_EDGE('',*,*,#3630,.F.);
#4742=ORIENTED_EDGE('',*,*,#3615,.F.);
#4743=ORIENTED_EDGE('',*,*,#3619,.F.);
#4744=ORIENTED_EDGE('',*,*,#3622,.F.);
#4745=ORIENTED_EDGE('',*,*,#3625,.F.);
#4746=ORIENTED_EDGE('',*,*,#3628,.F.);
#4747=ORIENTED_EDGE('',*,*,#3631,.T.);
#4748=ORIENTED_EDGE('',*,*,#3632,.F.);
#4749=ORIENTED_EDGE('',*,*,#3631,.F.);
#4750=ORIENTED_EDGE('',*,*,#3633,.T.);
#4751=ORIENTED_EDGE('',*,*,#3634,.T.);
#4752=ORIENTED_EDGE('',*,*,#3633,.F.);
#4753=ORIENTED_EDGE('',*,*,#3634,.F.);
#4754=ORIENTED_EDGE('',*,*,#3635,.F.);
#4755=ORIENTED_EDGE('',*,*,#3636,.F.);
#4756=ORIENTED_EDGE('',*,*,#3637,.T.);
#4757=ORIENTED_EDGE('',*,*,#3635,.T.);
#4758=ORIENTED_EDGE('',*,*,#3637,.F.);
#4759=ORIENTED_EDGE('',*,*,#3638,.F.);
#4760=ORIENTED_EDGE('',*,*,#3639,.T.);
#4761=ORIENTED_EDGE('',*,*,#3636,.T.);
#4762=ORIENTED_EDGE('',*,*,#3639,.F.);
#4763=ORIENTED_EDGE('',*,*,#3640,.F.);
#4764=ORIENTED_EDGE('',*,*,#3641,.T.);
#4765=ORIENTED_EDGE('',*,*,#3638,.T.);
#4766=ORIENTED_EDGE('',*,*,#3641,.F.);
#4767=ORIENTED_EDGE('',*,*,#3640,.T.);
#4768=ORIENTED_EDGE('',*,*,#3642,.F.);
#4769=ORIENTED_EDGE('',*,*,#3643,.F.);
#4770=ORIENTED_EDGE('',*,*,#3644,.T.);
#4771=ORIENTED_EDGE('',*,*,#3642,.T.);
#4772=ORIENTED_EDGE('',*,*,#3644,.F.);
#4773=ORIENTED_EDGE('',*,*,#3632,.T.);
#4774=ORIENTED_EDGE('',*,*,#3645,.T.);
#4775=ORIENTED_EDGE('',*,*,#3643,.T.);
#4776=ORIENTED_EDGE('',*,*,#3645,.F.);
#4777=ORIENTED_EDGE('',*,*,#3646,.T.);
#4778=ORIENTED_EDGE('',*,*,#3647,.T.);
#4779=ORIENTED_EDGE('',*,*,#3648,.T.);
#4780=ORIENTED_EDGE('',*,*,#3647,.F.);
#4781=ORIENTED_EDGE('',*,*,#3648,.F.);
#4782=ORIENTED_EDGE('',*,*,#3649,.T.);
#4783=ORIENTED_EDGE('',*,*,#3650,.T.);
#4784=ORIENTED_EDGE('',*,*,#3649,.F.);
#4785=ORIENTED_EDGE('',*,*,#3651,.T.);
#4786=ORIENTED_EDGE('',*,*,#3646,.F.);
#4787=ORIENTED_EDGE('',*,*,#3651,.F.);
#4788=ORIENTED_EDGE('',*,*,#3652,.T.);
#4789=ORIENTED_EDGE('',*,*,#3653,.T.);
#4790=ORIENTED_EDGE('',*,*,#3652,.F.);
#4791=ORIENTED_EDGE('',*,*,#3653,.F.);
#4792=ORIENTED_EDGE('',*,*,#3650,.F.);
#4793=ORIENTED_EDGE('',*,*,#3654,.F.);
#4794=ORIENTED_EDGE('',*,*,#3655,.F.);
#4795=ORIENTED_EDGE('',*,*,#3656,.T.);
#4796=ORIENTED_EDGE('',*,*,#3657,.F.);
#4797=ORIENTED_EDGE('',*,*,#3656,.F.);
#4798=ORIENTED_EDGE('',*,*,#3658,.F.);
#4799=ORIENTED_EDGE('',*,*,#3659,.F.);
#4800=ORIENTED_EDGE('',*,*,#3660,.F.);
#4801=ORIENTED_EDGE('',*,*,#3661,.F.);
#4802=ORIENTED_EDGE('',*,*,#3662,.F.);
#4803=ORIENTED_EDGE('',*,*,#3663,.T.);
#4804=ORIENTED_EDGE('',*,*,#3664,.F.);
#4805=ORIENTED_EDGE('',*,*,#3665,.F.);
#4806=ORIENTED_EDGE('',*,*,#3666,.F.);
#4807=ORIENTED_EDGE('',*,*,#3667,.F.);
#4808=ORIENTED_EDGE('',*,*,#3668,.F.);
#4809=ORIENTED_EDGE('',*,*,#3669,.F.);
#4810=ORIENTED_EDGE('',*,*,#3663,.F.);
#4811=ORIENTED_EDGE('',*,*,#3659,.T.);
#4812=ORIENTED_EDGE('',*,*,#3670,.T.);
#4813=ORIENTED_EDGE('',*,*,#3668,.T.);
#4814=ORIENTED_EDGE('',*,*,#3671,.F.);
#4815=ORIENTED_EDGE('',*,*,#3658,.T.);
#4816=ORIENTED_EDGE('',*,*,#3672,.T.);
#4817=ORIENTED_EDGE('',*,*,#3669,.T.);
#4818=ORIENTED_EDGE('',*,*,#3670,.F.);
#4819=ORIENTED_EDGE('',*,*,#3655,.T.);
#4820=ORIENTED_EDGE('',*,*,#3673,.T.);
#4821=ORIENTED_EDGE('',*,*,#3664,.T.);
#4822=ORIENTED_EDGE('',*,*,#3672,.F.);
#4823=ORIENTED_EDGE('',*,*,#3674,.F.);
#4824=ORIENTED_EDGE('',*,*,#3675,.T.);
#4825=ORIENTED_EDGE('',*,*,#3676,.T.);
#4826=ORIENTED_EDGE('',*,*,#3675,.F.);
#4827=ORIENTED_EDGE('',*,*,#3654,.T.);
#4828=ORIENTED_EDGE('',*,*,#3677,.T.);
#4829=ORIENTED_EDGE('',*,*,#3665,.T.);
#4830=ORIENTED_EDGE('',*,*,#3673,.F.);
#4831=ORIENTED_EDGE('',*,*,#3660,.T.);
#4832=ORIENTED_EDGE('',*,*,#3671,.T.);
#4833=ORIENTED_EDGE('',*,*,#3667,.T.);
#4834=ORIENTED_EDGE('',*,*,#3678,.F.);
#4835=ORIENTED_EDGE('',*,*,#3661,.T.);
#4836=ORIENTED_EDGE('',*,*,#3678,.T.);
#4837=ORIENTED_EDGE('',*,*,#3666,.T.);
#4838=ORIENTED_EDGE('',*,*,#3677,.F.);
#4839=ORIENTED_EDGE('',*,*,#3662,.T.);
#4840=ORIENTED_EDGE('',*,*,#3674,.T.);
#4841=ORIENTED_EDGE('',*,*,#3657,.T.);
#4842=ORIENTED_EDGE('',*,*,#3676,.F.);
#4843=ORIENTED_EDGE('',*,*,#3679,.T.);
#4844=ORIENTED_EDGE('',*,*,#3680,.T.);
#4845=ORIENTED_EDGE('',*,*,#3681,.T.);
#4846=ORIENTED_EDGE('',*,*,#3682,.T.);
#4847=ORIENTED_EDGE('',*,*,#3683,.T.);
#4848=ORIENTED_EDGE('',*,*,#3684,.T.);
#4849=ORIENTED_EDGE('',*,*,#3685,.F.);
#4850=ORIENTED_EDGE('',*,*,#3686,.T.);
#4851=ORIENTED_EDGE('',*,*,#3687,.T.);
#4852=ORIENTED_EDGE('',*,*,#3688,.T.);
#4853=ORIENTED_EDGE('',*,*,#3689,.T.);
#4854=ORIENTED_EDGE('',*,*,#3690,.T.);
#4855=ORIENTED_EDGE('',*,*,#3691,.T.);
#4856=ORIENTED_EDGE('',*,*,#3692,.F.);
#4857=ORIENTED_EDGE('',*,*,#3693,.F.);
#4858=ORIENTED_EDGE('',*,*,#3691,.F.);
#4859=ORIENTED_EDGE('',*,*,#3694,.F.);
#4860=ORIENTED_EDGE('',*,*,#3680,.F.);
#4861=ORIENTED_EDGE('',*,*,#3694,.T.);
#4862=ORIENTED_EDGE('',*,*,#3690,.F.);
#4863=ORIENTED_EDGE('',*,*,#3695,.F.);
#4864=ORIENTED_EDGE('',*,*,#3681,.F.);
#4865=ORIENTED_EDGE('',*,*,#3695,.T.);
#4866=ORIENTED_EDGE('',*,*,#3689,.F.);
#4867=ORIENTED_EDGE('',*,*,#3696,.F.);
#4868=ORIENTED_EDGE('',*,*,#3682,.F.);
#4869=ORIENTED_EDGE('',*,*,#3696,.T.);
#4870=ORIENTED_EDGE('',*,*,#3688,.F.);
#4871=ORIENTED_EDGE('',*,*,#3697,.F.);
#4872=ORIENTED_EDGE('',*,*,#3683,.F.);
#4873=ORIENTED_EDGE('',*,*,#3697,.T.);
#4874=ORIENTED_EDGE('',*,*,#3687,.F.);
#4875=ORIENTED_EDGE('',*,*,#3698,.F.);
#4876=ORIENTED_EDGE('',*,*,#3684,.F.);
#4877=ORIENTED_EDGE('',*,*,#3698,.T.);
#4878=ORIENTED_EDGE('',*,*,#3686,.F.);
#4879=ORIENTED_EDGE('',*,*,#3693,.T.);
#4880=ORIENTED_EDGE('',*,*,#3679,.F.);
#4881=ORIENTED_EDGE('',*,*,#3692,.T.);
#4882=ORIENTED_EDGE('',*,*,#3699,.T.);
#4883=ORIENTED_EDGE('',*,*,#3700,.T.);
#4884=ORIENTED_EDGE('',*,*,#3699,.F.);
#4885=ORIENTED_EDGE('',*,*,#3701,.F.);
#4886=ORIENTED_EDGE('',*,*,#3702,.T.);
#4887=ORIENTED_EDGE('',*,*,#3700,.F.);
#4888=ORIENTED_EDGE('',*,*,#3703,.T.);
#4889=ORIENTED_EDGE('',*,*,#3701,.T.);
#4890=ORIENTED_EDGE('',*,*,#3703,.F.);
#4891=ORIENTED_EDGE('',*,*,#3704,.F.);
#4892=ORIENTED_EDGE('',*,*,#3705,.T.);
#4893=ORIENTED_EDGE('',*,*,#3685,.T.);
#4894=ORIENTED_EDGE('',*,*,#3705,.F.);
#4895=ORIENTED_EDGE('',*,*,#3706,.F.);
#4896=ORIENTED_EDGE('',*,*,#3707,.T.);
#4897=ORIENTED_EDGE('',*,*,#3704,.T.);
#4898=ORIENTED_EDGE('',*,*,#3707,.F.);
#4899=ORIENTED_EDGE('',*,*,#3706,.T.);
#4900=ORIENTED_EDGE('',*,*,#3708,.F.);
#4901=ORIENTED_EDGE('',*,*,#3708,.T.);
#4902=ORIENTED_EDGE('',*,*,#3709,.T.);
#4903=ORIENTED_EDGE('',*,*,#3702,.F.);
#4904=ORIENTED_EDGE('',*,*,#3709,.F.);
#4905=ORIENTED_EDGE('',*,*,#3710,.F.);
#4906=ORIENTED_EDGE('',*,*,#3711,.T.);
#4907=ORIENTED_EDGE('',*,*,#3712,.T.);
#4908=ORIENTED_EDGE('',*,*,#3711,.F.);
#4909=ORIENTED_EDGE('',*,*,#3713,.F.);
#4910=ORIENTED_EDGE('',*,*,#3714,.T.);
#4911=ORIENTED_EDGE('',*,*,#3715,.T.);
#4912=ORIENTED_EDGE('',*,*,#3714,.F.);
#4913=ORIENTED_EDGE('',*,*,#3713,.T.);
#4914=ORIENTED_EDGE('',*,*,#3710,.T.);
#4915=ORIENTED_EDGE('',*,*,#3715,.F.);
#4916=ORIENTED_EDGE('',*,*,#3712,.F.);
#4917=ORIENTED_EDGE('',*,*,#3716,.F.);
#4918=ORIENTED_EDGE('',*,*,#3717,.F.);
#4919=ORIENTED_EDGE('',*,*,#3718,.T.);
#4920=ORIENTED_EDGE('',*,*,#3716,.T.);
#4921=ORIENTED_EDGE('',*,*,#3718,.F.);
#4922=ORIENTED_EDGE('',*,*,#3719,.F.);
#4923=ORIENTED_EDGE('',*,*,#3720,.T.);
#4924=ORIENTED_EDGE('',*,*,#3717,.T.);
#4925=ORIENTED_EDGE('',*,*,#3720,.F.);
#4926=ORIENTED_EDGE('',*,*,#3721,.F.);
#4927=ORIENTED_EDGE('',*,*,#3722,.T.);
#4928=ORIENTED_EDGE('',*,*,#3719,.T.);
#4929=ORIENTED_EDGE('',*,*,#3722,.F.);
#4930=ORIENTED_EDGE('',*,*,#3721,.T.);
#4931=ORIENTED_EDGE('',*,*,#3723,.F.);
#4932=ORIENTED_EDGE('',*,*,#3724,.F.);
#4933=ORIENTED_EDGE('',*,*,#3725,.T.);
#4934=ORIENTED_EDGE('',*,*,#3723,.T.);
#4935=ORIENTED_EDGE('',*,*,#3725,.F.);
#4936=ORIENTED_EDGE('',*,*,#3726,.F.);
#4937=ORIENTED_EDGE('',*,*,#3727,.T.);
#4938=ORIENTED_EDGE('',*,*,#3724,.T.);
#4939=ORIENTED_EDGE('',*,*,#3727,.F.);
#4940=ORIENTED_EDGE('',*,*,#3728,.F.);
#4941=ORIENTED_EDGE('',*,*,#3729,.T.);
#4942=ORIENTED_EDGE('',*,*,#3726,.T.);
#4943=ORIENTED_EDGE('',*,*,#3729,.F.);
#4944=ORIENTED_EDGE('',*,*,#3728,.T.);
#4945=ORIENTED_EDGE('',*,*,#3730,.T.);
#4946=ORIENTED_EDGE('',*,*,#3731,.T.);
#4947=ORIENTED_EDGE('',*,*,#3732,.T.);
#4948=ORIENTED_EDGE('',*,*,#3733,.F.);
#4949=ORIENTED_EDGE('',*,*,#3734,.T.);
#4950=ORIENTED_EDGE('',*,*,#3735,.T.);
#4951=ORIENTED_EDGE('',*,*,#3736,.T.);
#4952=ORIENTED_EDGE('',*,*,#3731,.F.);
#4953=ORIENTED_EDGE('',*,*,#3737,.T.);
#4954=ORIENTED_EDGE('',*,*,#3738,.T.);
#4955=ORIENTED_EDGE('',*,*,#3739,.T.);
#4956=ORIENTED_EDGE('',*,*,#3735,.F.);
#4957=ORIENTED_EDGE('',*,*,#3740,.T.);
#4958=ORIENTED_EDGE('',*,*,#3741,.T.);
#4959=ORIENTED_EDGE('',*,*,#3742,.T.);
#4960=ORIENTED_EDGE('',*,*,#3738,.F.);
#4961=ORIENTED_EDGE('',*,*,#3743,.T.);
#4962=ORIENTED_EDGE('',*,*,#3744,.T.);
#4963=ORIENTED_EDGE('',*,*,#3745,.T.);
#4964=ORIENTED_EDGE('',*,*,#3741,.F.);
#4965=ORIENTED_EDGE('',*,*,#3746,.T.);
#4966=ORIENTED_EDGE('',*,*,#3733,.T.);
#4967=ORIENTED_EDGE('',*,*,#3747,.T.);
#4968=ORIENTED_EDGE('',*,*,#3744,.F.);
#4969=ORIENTED_EDGE('',*,*,#3746,.F.);
#4970=ORIENTED_EDGE('',*,*,#3743,.F.);
#4971=ORIENTED_EDGE('',*,*,#3740,.F.);
#4972=ORIENTED_EDGE('',*,*,#3737,.F.);
#4973=ORIENTED_EDGE('',*,*,#3734,.F.);
#4974=ORIENTED_EDGE('',*,*,#3730,.F.);
#4975=ORIENTED_EDGE('',*,*,#3747,.F.);
#4976=ORIENTED_EDGE('',*,*,#3732,.F.);
#4977=ORIENTED_EDGE('',*,*,#3736,.F.);
#4978=ORIENTED_EDGE('',*,*,#3739,.F.);
#4979=ORIENTED_EDGE('',*,*,#3742,.F.);
#4980=ORIENTED_EDGE('',*,*,#3745,.F.);
#4981=ORIENTED_EDGE('',*,*,#3748,.F.);
#4982=ORIENTED_EDGE('',*,*,#3749,.T.);
#4983=ORIENTED_EDGE('',*,*,#3750,.T.);
#4984=ORIENTED_EDGE('',*,*,#3749,.F.);
#4985=ORIENTED_EDGE('',*,*,#3748,.T.);
#4986=ORIENTED_EDGE('',*,*,#3750,.F.);
#4987=ORIENTED_EDGE('',*,*,#3751,.F.);
#4988=ORIENTED_EDGE('',*,*,#3752,.F.);
#4989=ORIENTED_EDGE('',*,*,#3753,.T.);
#4990=ORIENTED_EDGE('',*,*,#3754,.F.);
#4991=ORIENTED_EDGE('',*,*,#3753,.F.);
#4992=ORIENTED_EDGE('',*,*,#3755,.F.);
#4993=ORIENTED_EDGE('',*,*,#3756,.T.);
#4994=ORIENTED_EDGE('',*,*,#3756,.F.);
#4995=ORIENTED_EDGE('',*,*,#3755,.T.);
#4996=ORIENTED_EDGE('',*,*,#3752,.T.);
#4997=ORIENTED_EDGE('',*,*,#3757,.T.);
#4998=ORIENTED_EDGE('',*,*,#3758,.T.);
#4999=ORIENTED_EDGE('',*,*,#3751,.T.);
#5000=ORIENTED_EDGE('',*,*,#3758,.F.);
#5001=ORIENTED_EDGE('',*,*,#3759,.T.);
#5002=ORIENTED_EDGE('',*,*,#3760,.F.);
#5003=ORIENTED_EDGE('',*,*,#3759,.F.);
#5004=ORIENTED_EDGE('',*,*,#3757,.F.);
#5005=ORIENTED_EDGE('',*,*,#3761,.F.);
#5006=ORIENTED_EDGE('',*,*,#3754,.T.);
#5007=ORIENTED_EDGE('',*,*,#3762,.F.);
#5008=ORIENTED_EDGE('',*,*,#3763,.T.);
#5009=ORIENTED_EDGE('',*,*,#3761,.T.);
#5010=ORIENTED_EDGE('',*,*,#3763,.F.);
#5011=ORIENTED_EDGE('',*,*,#3764,.F.);
#5012=ORIENTED_EDGE('',*,*,#3765,.T.);
#5013=ORIENTED_EDGE('',*,*,#3766,.F.);
#5014=ORIENTED_EDGE('',*,*,#3765,.F.);
#5015=ORIENTED_EDGE('',*,*,#3764,.T.);
#5016=ORIENTED_EDGE('',*,*,#3760,.T.);
#5017=ORIENTED_EDGE('',*,*,#3767,.T.);
#5018=ORIENTED_EDGE('',*,*,#3768,.T.);
#5019=ORIENTED_EDGE('',*,*,#3769,.F.);
#5020=ORIENTED_EDGE('',*,*,#3770,.F.);
#5021=ORIENTED_EDGE('',*,*,#3771,.F.);
#5022=ORIENTED_EDGE('',*,*,#3768,.F.);
#5023=ORIENTED_EDGE('',*,*,#3772,.T.);
#5024=ORIENTED_EDGE('',*,*,#3773,.T.);
#5025=ORIENTED_EDGE('',*,*,#3772,.F.);
#5026=ORIENTED_EDGE('',*,*,#3767,.F.);
#5027=ORIENTED_EDGE('',*,*,#3774,.F.);
#5028=ORIENTED_EDGE('',*,*,#3762,.T.);
#5029=ORIENTED_EDGE('',*,*,#3775,.F.);
#5030=ORIENTED_EDGE('',*,*,#3776,.T.);
#5031=ORIENTED_EDGE('',*,*,#3774,.T.);
#5032=ORIENTED_EDGE('',*,*,#3776,.F.);
#5033=ORIENTED_EDGE('',*,*,#3775,.T.);
#5034=ORIENTED_EDGE('',*,*,#3773,.F.);
#5035=ORIENTED_EDGE('',*,*,#3777,.F.);
#5036=ORIENTED_EDGE('',*,*,#3778,.T.);
#5037=ORIENTED_EDGE('',*,*,#3779,.F.);
#5038=ORIENTED_EDGE('',*,*,#3780,.T.);
#5039=ORIENTED_EDGE('',*,*,#3777,.T.);
#5040=ORIENTED_EDGE('',*,*,#3780,.F.);
#5041=ORIENTED_EDGE('',*,*,#3779,.T.);
#5042=ORIENTED_EDGE('',*,*,#3766,.T.);
#5043=ORIENTED_EDGE('',*,*,#3778,.F.);
#5044=ORIENTED_EDGE('',*,*,#3781,.T.);
#5045=ORIENTED_EDGE('',*,*,#3769,.T.);
#5046=ORIENTED_EDGE('',*,*,#3771,.T.);
#5047=ORIENTED_EDGE('',*,*,#3770,.T.);
#5048=ORIENTED_EDGE('',*,*,#3781,.F.);
#5049=ORIENTED_EDGE('',*,*,#3782,.T.);
#5050=ORIENTED_EDGE('',*,*,#3783,.T.);
#5051=ORIENTED_EDGE('',*,*,#3784,.T.);
#5052=ORIENTED_EDGE('',*,*,#3785,.T.);
#5053=ORIENTED_EDGE('',*,*,#3786,.T.);
#5054=ORIENTED_EDGE('',*,*,#3787,.T.);
#5055=ORIENTED_EDGE('',*,*,#3788,.F.);
#5056=ORIENTED_EDGE('',*,*,#3789,.T.);
#5057=ORIENTED_EDGE('',*,*,#3790,.T.);
#5058=ORIENTED_EDGE('',*,*,#3791,.T.);
#5059=ORIENTED_EDGE('',*,*,#3792,.T.);
#5060=ORIENTED_EDGE('',*,*,#3793,.T.);
#5061=ORIENTED_EDGE('',*,*,#3794,.T.);
#5062=ORIENTED_EDGE('',*,*,#3795,.F.);
#5063=ORIENTED_EDGE('',*,*,#3796,.F.);
#5064=ORIENTED_EDGE('',*,*,#3794,.F.);
#5065=ORIENTED_EDGE('',*,*,#3797,.F.);
#5066=ORIENTED_EDGE('',*,*,#3783,.F.);
#5067=ORIENTED_EDGE('',*,*,#3797,.T.);
#5068=ORIENTED_EDGE('',*,*,#3793,.F.);
#5069=ORIENTED_EDGE('',*,*,#3798,.F.);
#5070=ORIENTED_EDGE('',*,*,#3784,.F.);
#5071=ORIENTED_EDGE('',*,*,#3798,.T.);
#5072=ORIENTED_EDGE('',*,*,#3792,.F.);
#5073=ORIENTED_EDGE('',*,*,#3799,.F.);
#5074=ORIENTED_EDGE('',*,*,#3785,.F.);
#5075=ORIENTED_EDGE('',*,*,#3799,.T.);
#5076=ORIENTED_EDGE('',*,*,#3791,.F.);
#5077=ORIENTED_EDGE('',*,*,#3800,.F.);
#5078=ORIENTED_EDGE('',*,*,#3786,.F.);
#5079=ORIENTED_EDGE('',*,*,#3800,.T.);
#5080=ORIENTED_EDGE('',*,*,#3790,.F.);
#5081=ORIENTED_EDGE('',*,*,#3801,.F.);
#5082=ORIENTED_EDGE('',*,*,#3787,.F.);
#5083=ORIENTED_EDGE('',*,*,#3801,.T.);
#5084=ORIENTED_EDGE('',*,*,#3789,.F.);
#5085=ORIENTED_EDGE('',*,*,#3796,.T.);
#5086=ORIENTED_EDGE('',*,*,#3782,.F.);
#5087=ORIENTED_EDGE('',*,*,#3795,.T.);
#5088=ORIENTED_EDGE('',*,*,#3802,.T.);
#5089=ORIENTED_EDGE('',*,*,#3803,.T.);
#5090=ORIENTED_EDGE('',*,*,#3802,.F.);
#5091=ORIENTED_EDGE('',*,*,#3804,.F.);
#5092=ORIENTED_EDGE('',*,*,#3805,.T.);
#5093=ORIENTED_EDGE('',*,*,#3803,.F.);
#5094=ORIENTED_EDGE('',*,*,#3806,.T.);
#5095=ORIENTED_EDGE('',*,*,#3804,.T.);
#5096=ORIENTED_EDGE('',*,*,#3806,.F.);
#5097=ORIENTED_EDGE('',*,*,#3807,.F.);
#5098=ORIENTED_EDGE('',*,*,#3808,.T.);
#5099=ORIENTED_EDGE('',*,*,#3788,.T.);
#5100=ORIENTED_EDGE('',*,*,#3808,.F.);
#5101=ORIENTED_EDGE('',*,*,#3809,.F.);
#5102=ORIENTED_EDGE('',*,*,#3810,.T.);
#5103=ORIENTED_EDGE('',*,*,#3807,.T.);
#5104=ORIENTED_EDGE('',*,*,#3810,.F.);
#5105=ORIENTED_EDGE('',*,*,#3809,.T.);
#5106=ORIENTED_EDGE('',*,*,#3811,.F.);
#5107=ORIENTED_EDGE('',*,*,#3811,.T.);
#5108=ORIENTED_EDGE('',*,*,#3812,.T.);
#5109=ORIENTED_EDGE('',*,*,#3805,.F.);
#5110=ORIENTED_EDGE('',*,*,#3812,.F.);
#5111=ORIENTED_EDGE('',*,*,#3813,.F.);
#5112=ORIENTED_EDGE('',*,*,#3814,.T.);
#5113=ORIENTED_EDGE('',*,*,#3815,.F.);
#5114=ORIENTED_EDGE('',*,*,#3814,.F.);
#5115=ORIENTED_EDGE('',*,*,#3816,.F.);
#5116=ORIENTED_EDGE('',*,*,#3817,.T.);
#5117=ORIENTED_EDGE('',*,*,#3813,.T.);
#5118=ORIENTED_EDGE('',*,*,#3817,.F.);
#5119=ORIENTED_EDGE('',*,*,#3816,.T.);
#5120=ORIENTED_EDGE('',*,*,#3818,.F.);
#5121=ORIENTED_EDGE('',*,*,#3819,.T.);
#5122=ORIENTED_EDGE('',*,*,#3820,.F.);
#5123=ORIENTED_EDGE('',*,*,#3821,.F.);
#5124=ORIENTED_EDGE('',*,*,#3822,.F.);
#5125=ORIENTED_EDGE('',*,*,#3823,.F.);
#5126=ORIENTED_EDGE('',*,*,#3824,.F.);
#5127=ORIENTED_EDGE('',*,*,#3825,.F.);
#5128=ORIENTED_EDGE('',*,*,#3819,.F.);
#5129=ORIENTED_EDGE('',*,*,#3824,.T.);
#5130=ORIENTED_EDGE('',*,*,#3826,.F.);
#5131=ORIENTED_EDGE('',*,*,#3827,.T.);
#5132=ORIENTED_EDGE('',*,*,#3828,.T.);
#5133=ORIENTED_EDGE('',*,*,#3823,.T.);
#5134=ORIENTED_EDGE('',*,*,#3829,.F.);
#5135=ORIENTED_EDGE('',*,*,#3830,.T.);
#5136=ORIENTED_EDGE('',*,*,#3826,.T.);
#5137=ORIENTED_EDGE('',*,*,#3822,.T.);
#5138=ORIENTED_EDGE('',*,*,#3831,.F.);
#5139=ORIENTED_EDGE('',*,*,#3832,.T.);
#5140=ORIENTED_EDGE('',*,*,#3829,.T.);
#5141=ORIENTED_EDGE('',*,*,#3821,.T.);
#5142=ORIENTED_EDGE('',*,*,#3833,.F.);
#5143=ORIENTED_EDGE('',*,*,#3834,.T.);
#5144=ORIENTED_EDGE('',*,*,#3831,.T.);
#5145=ORIENTED_EDGE('',*,*,#3820,.T.);
#5146=ORIENTED_EDGE('',*,*,#3835,.F.);
#5147=ORIENTED_EDGE('',*,*,#3836,.T.);
#5148=ORIENTED_EDGE('',*,*,#3833,.T.);
#5149=ORIENTED_EDGE('',*,*,#3825,.T.);
#5150=ORIENTED_EDGE('',*,*,#3828,.F.);
#5151=ORIENTED_EDGE('',*,*,#3837,.T.);
#5152=ORIENTED_EDGE('',*,*,#3835,.T.);
#5153=ORIENTED_EDGE('',*,*,#3818,.T.);
#5154=ORIENTED_EDGE('',*,*,#3832,.F.);
#5155=ORIENTED_EDGE('',*,*,#3834,.F.);
#5156=ORIENTED_EDGE('',*,*,#3836,.F.);
#5157=ORIENTED_EDGE('',*,*,#3837,.F.);
#5158=ORIENTED_EDGE('',*,*,#3827,.F.);
#5159=ORIENTED_EDGE('',*,*,#3830,.F.);
#5160=ORIENTED_EDGE('',*,*,#3815,.T.);
#5161=ORIENTED_EDGE('',*,*,#3838,.F.);
#5162=ORIENTED_EDGE('',*,*,#3839,.F.);
#5163=ORIENTED_EDGE('',*,*,#3840,.F.);
#5164=ORIENTED_EDGE('',*,*,#3841,.T.);
#5165=ORIENTED_EDGE('',*,*,#3842,.F.);
#5166=ORIENTED_EDGE('',*,*,#3841,.F.);
#5167=ORIENTED_EDGE('',*,*,#3843,.F.);
#5168=ORIENTED_EDGE('',*,*,#3844,.T.);
#5169=ORIENTED_EDGE('',*,*,#3845,.F.);
#5170=ORIENTED_EDGE('',*,*,#3846,.F.);
#5171=ORIENTED_EDGE('',*,*,#3844,.F.);
#5172=ORIENTED_EDGE('',*,*,#3847,.F.);
#5173=ORIENTED_EDGE('',*,*,#3848,.T.);
#5174=ORIENTED_EDGE('',*,*,#3849,.F.);
#5175=ORIENTED_EDGE('',*,*,#3848,.F.);
#5176=ORIENTED_EDGE('',*,*,#3850,.F.);
#5177=ORIENTED_EDGE('',*,*,#3839,.T.);
#5178=ORIENTED_EDGE('',*,*,#3843,.T.);
#5179=ORIENTED_EDGE('',*,*,#3840,.T.);
#5180=ORIENTED_EDGE('',*,*,#3850,.T.);
#5181=ORIENTED_EDGE('',*,*,#3847,.T.);
#5182=ORIENTED_EDGE('',*,*,#3851,.F.);
#5183=ORIENTED_EDGE('',*,*,#3852,.T.);
#5184=ORIENTED_EDGE('',*,*,#3853,.F.);
#5185=ORIENTED_EDGE('',*,*,#3852,.F.);
#5186=ORIENTED_EDGE('',*,*,#3846,.T.);
#5187=ORIENTED_EDGE('',*,*,#3849,.T.);
#5188=ORIENTED_EDGE('',*,*,#3838,.T.);
#5189=ORIENTED_EDGE('',*,*,#3842,.T.);
#5190=ORIENTED_EDGE('',*,*,#3854,.T.);
#5191=ORIENTED_EDGE('',*,*,#3854,.F.);
#5192=ORIENTED_EDGE('',*,*,#3845,.T.);
#5193=ORIENTED_EDGE('',*,*,#3853,.T.);
#5194=ORIENTED_EDGE('',*,*,#3851,.T.);
#5195=ORIENTED_EDGE('',*,*,#3855,.F.);
#5196=ORIENTED_EDGE('',*,*,#3856,.T.);
#5197=ORIENTED_EDGE('',*,*,#3857,.F.);
#5198=ORIENTED_EDGE('',*,*,#3856,.F.);
#5199=ORIENTED_EDGE('',*,*,#3855,.T.);
#5200=ORIENTED_EDGE('',*,*,#3858,.T.);
#5201=ORIENTED_EDGE('',*,*,#3859,.F.);
#5202=ORIENTED_EDGE('',*,*,#3860,.F.);
#5203=ORIENTED_EDGE('',*,*,#3861,.T.);
#5204=ORIENTED_EDGE('',*,*,#3862,.F.);
#5205=ORIENTED_EDGE('',*,*,#3863,.F.);
#5206=ORIENTED_EDGE('',*,*,#3864,.T.);
#5207=ORIENTED_EDGE('',*,*,#3865,.F.);
#5208=ORIENTED_EDGE('',*,*,#3866,.F.);
#5209=ORIENTED_EDGE('',*,*,#3867,.T.);
#5210=ORIENTED_EDGE('',*,*,#3868,.F.);
#5211=ORIENTED_EDGE('',*,*,#3869,.F.);
#5212=ORIENTED_EDGE('',*,*,#3868,.T.);
#5213=ORIENTED_EDGE('',*,*,#3870,.F.);
#5214=ORIENTED_EDGE('',*,*,#3860,.T.);
#5215=ORIENTED_EDGE('',*,*,#3871,.T.);
#5216=ORIENTED_EDGE('',*,*,#3872,.F.);
#5217=ORIENTED_EDGE('',*,*,#3873,.F.);
#5218=ORIENTED_EDGE('',*,*,#3865,.T.);
#5219=ORIENTED_EDGE('',*,*,#3874,.F.);
#5220=ORIENTED_EDGE('',*,*,#3869,.T.);
#5221=ORIENTED_EDGE('',*,*,#3873,.T.);
#5222=ORIENTED_EDGE('',*,*,#3875,.F.);
#5223=ORIENTED_EDGE('',*,*,#3876,.F.);
#5224=ORIENTED_EDGE('',*,*,#3862,.T.);
#5225=ORIENTED_EDGE('',*,*,#3877,.F.);
#5226=ORIENTED_EDGE('',*,*,#3866,.T.);
#5227=ORIENTED_EDGE('',*,*,#3876,.T.);
#5228=ORIENTED_EDGE('',*,*,#3878,.F.);
#5229=ORIENTED_EDGE('',*,*,#3879,.F.);
#5230=ORIENTED_EDGE('',*,*,#3859,.T.);
#5231=ORIENTED_EDGE('',*,*,#3880,.F.);
#5232=ORIENTED_EDGE('',*,*,#3863,.T.);
#5233=ORIENTED_EDGE('',*,*,#3879,.T.);
#5234=ORIENTED_EDGE('',*,*,#3881,.F.);
#5235=ORIENTED_EDGE('',*,*,#3871,.F.);
#5236=ORIENTED_EDGE('',*,*,#3881,.T.);
#5237=ORIENTED_EDGE('',*,*,#3878,.T.);
#5238=ORIENTED_EDGE('',*,*,#3875,.T.);
#5239=ORIENTED_EDGE('',*,*,#3872,.T.);
#5240=ORIENTED_EDGE('',*,*,#3857,.T.);
#5241=ORIENTED_EDGE('',*,*,#3877,.T.);
#5242=ORIENTED_EDGE('',*,*,#3882,.T.);
#5243=ORIENTED_EDGE('',*,*,#3880,.T.);
#5244=ORIENTED_EDGE('',*,*,#3883,.T.);
#5245=ORIENTED_EDGE('',*,*,#3884,.T.);
#5246=ORIENTED_EDGE('',*,*,#3870,.T.);
#5247=ORIENTED_EDGE('',*,*,#3885,.T.);
#5248=ORIENTED_EDGE('',*,*,#3874,.T.);
#5249=ORIENTED_EDGE('',*,*,#3886,.T.);
#5250=ORIENTED_EDGE('',*,*,#3887,.T.);
#5251=ORIENTED_EDGE('',*,*,#3888,.T.);
#5252=ORIENTED_EDGE('',*,*,#3889,.F.);
#5253=ORIENTED_EDGE('',*,*,#3890,.F.);
#5254=ORIENTED_EDGE('',*,*,#3891,.T.);
#5255=ORIENTED_EDGE('',*,*,#3890,.T.);
#5256=ORIENTED_EDGE('',*,*,#3892,.F.);
#5257=ORIENTED_EDGE('',*,*,#3893,.F.);
#5258=ORIENTED_EDGE('',*,*,#3894,.T.);
#5259=ORIENTED_EDGE('',*,*,#3893,.T.);
#5260=ORIENTED_EDGE('',*,*,#3895,.F.);
#5261=ORIENTED_EDGE('',*,*,#3896,.F.);
#5262=ORIENTED_EDGE('',*,*,#3897,.T.);
#5263=ORIENTED_EDGE('',*,*,#3896,.T.);
#5264=ORIENTED_EDGE('',*,*,#3898,.F.);
#5265=ORIENTED_EDGE('',*,*,#3888,.F.);
#5266=ORIENTED_EDGE('',*,*,#3897,.F.);
#5267=ORIENTED_EDGE('',*,*,#3887,.F.);
#5268=ORIENTED_EDGE('',*,*,#3891,.F.);
#5269=ORIENTED_EDGE('',*,*,#3894,.F.);
#5270=ORIENTED_EDGE('',*,*,#3883,.F.);
#5271=ORIENTED_EDGE('',*,*,#3858,.F.);
#5272=ORIENTED_EDGE('',*,*,#3885,.F.);
#5273=ORIENTED_EDGE('',*,*,#3867,.F.);
#5274=ORIENTED_EDGE('',*,*,#3886,.F.);
#5275=ORIENTED_EDGE('',*,*,#3864,.F.);
#5276=ORIENTED_EDGE('',*,*,#3882,.F.);
#5277=ORIENTED_EDGE('',*,*,#3861,.F.);
#5278=ORIENTED_EDGE('',*,*,#3884,.F.);
#5279=ORIENTED_EDGE('',*,*,#3899,.T.);
#5280=ORIENTED_EDGE('',*,*,#3900,.T.);
#5281=ORIENTED_EDGE('',*,*,#3899,.F.);
#5282=ORIENTED_EDGE('',*,*,#3900,.F.);
#5283=ORIENTED_EDGE('',*,*,#3889,.T.);
#5284=ORIENTED_EDGE('',*,*,#3898,.T.);
#5285=ORIENTED_EDGE('',*,*,#3895,.T.);
#5286=ORIENTED_EDGE('',*,*,#3892,.T.);
#5287=ORIENTED_EDGE('',*,*,#3901,.F.);
#5288=ORIENTED_EDGE('',*,*,#3902,.F.);
#5289=ORIENTED_EDGE('',*,*,#3903,.F.);
#5290=ORIENTED_EDGE('',*,*,#3904,.T.);
#5291=ORIENTED_EDGE('',*,*,#3905,.F.);
#5292=ORIENTED_EDGE('',*,*,#3904,.F.);
#5293=ORIENTED_EDGE('',*,*,#3906,.F.);
#5294=ORIENTED_EDGE('',*,*,#3907,.T.);
#5295=ORIENTED_EDGE('',*,*,#3908,.F.);
#5296=ORIENTED_EDGE('',*,*,#3907,.F.);
#5297=ORIENTED_EDGE('',*,*,#3909,.F.);
#5298=ORIENTED_EDGE('',*,*,#3910,.T.);
#5299=ORIENTED_EDGE('',*,*,#3911,.F.);
#5300=ORIENTED_EDGE('',*,*,#3910,.F.);
#5301=ORIENTED_EDGE('',*,*,#3912,.F.);
#5302=ORIENTED_EDGE('',*,*,#3902,.T.);
#5303=ORIENTED_EDGE('',*,*,#3913,.T.);
#5304=ORIENTED_EDGE('',*,*,#3914,.T.);
#5305=ORIENTED_EDGE('',*,*,#3915,.F.);
#5306=ORIENTED_EDGE('',*,*,#3916,.F.);
#5307=ORIENTED_EDGE('',*,*,#3917,.T.);
#5308=ORIENTED_EDGE('',*,*,#3916,.T.);
#5309=ORIENTED_EDGE('',*,*,#3918,.F.);
#5310=ORIENTED_EDGE('',*,*,#3919,.F.);
#5311=ORIENTED_EDGE('',*,*,#3920,.T.);
#5312=ORIENTED_EDGE('',*,*,#3919,.T.);
#5313=ORIENTED_EDGE('',*,*,#3921,.F.);
#5314=ORIENTED_EDGE('',*,*,#3922,.F.);
#5315=ORIENTED_EDGE('',*,*,#3923,.T.);
#5316=ORIENTED_EDGE('',*,*,#3922,.T.);
#5317=ORIENTED_EDGE('',*,*,#3924,.F.);
#5318=ORIENTED_EDGE('',*,*,#3914,.F.);
#5319=ORIENTED_EDGE('',*,*,#3924,.T.);
#5320=ORIENTED_EDGE('',*,*,#3921,.T.);
#5321=ORIENTED_EDGE('',*,*,#3918,.T.);
#5322=ORIENTED_EDGE('',*,*,#3915,.T.);
#5323=ORIENTED_EDGE('',*,*,#3908,.T.);
#5324=ORIENTED_EDGE('',*,*,#3911,.T.);
#5325=ORIENTED_EDGE('',*,*,#3901,.T.);
#5326=ORIENTED_EDGE('',*,*,#3905,.T.);
#5327=ORIENTED_EDGE('',*,*,#3923,.F.);
#5328=ORIENTED_EDGE('',*,*,#3913,.F.);
#5329=ORIENTED_EDGE('',*,*,#3917,.F.);
#5330=ORIENTED_EDGE('',*,*,#3920,.F.);
#5331=ORIENTED_EDGE('',*,*,#3909,.T.);
#5332=ORIENTED_EDGE('',*,*,#3906,.T.);
#5333=ORIENTED_EDGE('',*,*,#3903,.T.);
#5334=ORIENTED_EDGE('',*,*,#3912,.T.);
#5335=ORIENTED_EDGE('',*,*,#3925,.F.);
#5336=ORIENTED_EDGE('',*,*,#3926,.T.);
#5337=ORIENTED_EDGE('',*,*,#3927,.T.);
#5338=ORIENTED_EDGE('',*,*,#3926,.F.);
#5339=ORIENTED_EDGE('',*,*,#3928,.F.);
#5340=ORIENTED_EDGE('',*,*,#3929,.T.);
#5341=ORIENTED_EDGE('',*,*,#3930,.T.);
#5342=ORIENTED_EDGE('',*,*,#3929,.F.);
#5343=ORIENTED_EDGE('',*,*,#3928,.T.);
#5344=ORIENTED_EDGE('',*,*,#3925,.T.);
#5345=ORIENTED_EDGE('',*,*,#3930,.F.);
#5346=ORIENTED_EDGE('',*,*,#3927,.F.);
#5347=ORIENTED_EDGE('',*,*,#3931,.T.);
#5348=ORIENTED_EDGE('',*,*,#3932,.T.);
#5349=ORIENTED_EDGE('',*,*,#3933,.F.);
#5350=ORIENTED_EDGE('',*,*,#3934,.F.);
#5351=ORIENTED_EDGE('',*,*,#3935,.T.);
#5352=ORIENTED_EDGE('',*,*,#3934,.T.);
#5353=ORIENTED_EDGE('',*,*,#3936,.F.);
#5354=ORIENTED_EDGE('',*,*,#3937,.F.);
#5355=ORIENTED_EDGE('',*,*,#3938,.T.);
#5356=ORIENTED_EDGE('',*,*,#3937,.T.);
#5357=ORIENTED_EDGE('',*,*,#3939,.F.);
#5358=ORIENTED_EDGE('',*,*,#3940,.F.);
#5359=ORIENTED_EDGE('',*,*,#3941,.T.);
#5360=ORIENTED_EDGE('',*,*,#3940,.T.);
#5361=ORIENTED_EDGE('',*,*,#3942,.F.);
#5362=ORIENTED_EDGE('',*,*,#3932,.F.);
#5363=ORIENTED_EDGE('',*,*,#3942,.T.);
#5364=ORIENTED_EDGE('',*,*,#3939,.T.);
#5365=ORIENTED_EDGE('',*,*,#3936,.T.);
#5366=ORIENTED_EDGE('',*,*,#3933,.T.);
#5367=ORIENTED_EDGE('',*,*,#3941,.F.);
#5368=ORIENTED_EDGE('',*,*,#3931,.F.);
#5369=ORIENTED_EDGE('',*,*,#3935,.F.);
#5370=ORIENTED_EDGE('',*,*,#3938,.F.);
#5371=ORIENTED_EDGE('',*,*,#3943,.T.);
#5372=ORIENTED_EDGE('',*,*,#3944,.T.);
#5373=ORIENTED_EDGE('',*,*,#3945,.T.);
#5374=ORIENTED_EDGE('',*,*,#3946,.F.);
#5375=ORIENTED_EDGE('',*,*,#3947,.T.);
#5376=ORIENTED_EDGE('',*,*,#3948,.T.);
#5377=ORIENTED_EDGE('',*,*,#3949,.T.);
#5378=ORIENTED_EDGE('',*,*,#3944,.F.);
#5379=ORIENTED_EDGE('',*,*,#3950,.T.);
#5380=ORIENTED_EDGE('',*,*,#3951,.T.);
#5381=ORIENTED_EDGE('',*,*,#3952,.T.);
#5382=ORIENTED_EDGE('',*,*,#3948,.F.);
#5383=ORIENTED_EDGE('',*,*,#3953,.T.);
#5384=ORIENTED_EDGE('',*,*,#3954,.T.);
#5385=ORIENTED_EDGE('',*,*,#3955,.T.);
#5386=ORIENTED_EDGE('',*,*,#3951,.F.);
#5387=ORIENTED_EDGE('',*,*,#3956,.T.);
#5388=ORIENTED_EDGE('',*,*,#3957,.T.);
#5389=ORIENTED_EDGE('',*,*,#3958,.T.);
#5390=ORIENTED_EDGE('',*,*,#3954,.F.);
#5391=ORIENTED_EDGE('',*,*,#3959,.T.);
#5392=ORIENTED_EDGE('',*,*,#3946,.T.);
#5393=ORIENTED_EDGE('',*,*,#3960,.T.);
#5394=ORIENTED_EDGE('',*,*,#3957,.F.);
#5395=ORIENTED_EDGE('',*,*,#3959,.F.);
#5396=ORIENTED_EDGE('',*,*,#3956,.F.);
#5397=ORIENTED_EDGE('',*,*,#3953,.F.);
#5398=ORIENTED_EDGE('',*,*,#3950,.F.);
#5399=ORIENTED_EDGE('',*,*,#3947,.F.);
#5400=ORIENTED_EDGE('',*,*,#3943,.F.);
#5401=ORIENTED_EDGE('',*,*,#3960,.F.);
#5402=ORIENTED_EDGE('',*,*,#3945,.F.);
#5403=ORIENTED_EDGE('',*,*,#3949,.F.);
#5404=ORIENTED_EDGE('',*,*,#3952,.F.);
#5405=ORIENTED_EDGE('',*,*,#3955,.F.);
#5406=ORIENTED_EDGE('',*,*,#3958,.F.);
#5407=ORIENTED_EDGE('',*,*,#3961,.F.);
#5408=ORIENTED_EDGE('',*,*,#3962,.F.);
#5409=ORIENTED_EDGE('',*,*,#3963,.F.);
#5410=ORIENTED_EDGE('',*,*,#3964,.T.);
#5411=ORIENTED_EDGE('',*,*,#3962,.T.);
#5412=ORIENTED_EDGE('',*,*,#3964,.F.);
#5413=ORIENTED_EDGE('',*,*,#3965,.F.);
#5414=ORIENTED_EDGE('',*,*,#3966,.T.);
#5415=ORIENTED_EDGE('',*,*,#3963,.T.);
#5416=ORIENTED_EDGE('',*,*,#3966,.F.);
#5417=ORIENTED_EDGE('',*,*,#3967,.F.);
#5418=ORIENTED_EDGE('',*,*,#3968,.T.);
#5419=ORIENTED_EDGE('',*,*,#3965,.T.);
#5420=ORIENTED_EDGE('',*,*,#3968,.F.);
#5421=ORIENTED_EDGE('',*,*,#3967,.T.);
#5422=ORIENTED_EDGE('',*,*,#3969,.F.);
#5423=ORIENTED_EDGE('',*,*,#3970,.F.);
#5424=ORIENTED_EDGE('',*,*,#3971,.T.);
#5425=ORIENTED_EDGE('',*,*,#3969,.T.);
#5426=ORIENTED_EDGE('',*,*,#3971,.F.);
#5427=ORIENTED_EDGE('',*,*,#3961,.T.);
#5428=ORIENTED_EDGE('',*,*,#3972,.T.);
#5429=ORIENTED_EDGE('',*,*,#3970,.T.);
#5430=ORIENTED_EDGE('',*,*,#3972,.F.);
#5431=CYLINDRICAL_SURFACE('',#6238,0.685);
#5432=CYLINDRICAL_SURFACE('',#6243,1.065);
#5433=CYLINDRICAL_SURFACE('',#6248,0.46);
#5434=CYLINDRICAL_SURFACE('',#6249,1.5);
#5435=CYLINDRICAL_SURFACE('',#6255,0.685);
#5436=CYLINDRICAL_SURFACE('',#6260,1.065);
#5437=CYLINDRICAL_SURFACE('',#6265,0.46);
#5438=CYLINDRICAL_SURFACE('',#6266,1.5);
#5439=CYLINDRICAL_SURFACE('',#6272,0.33);
#5440=CYLINDRICAL_SURFACE('',#6275,0.33);
#5441=CYLINDRICAL_SURFACE('',#6278,0.33);
#5442=CYLINDRICAL_SURFACE('',#6281,0.33);
#5443=CYLINDRICAL_SURFACE('',#6284,0.7);
#5444=CYLINDRICAL_SURFACE('',#6287,1.1);
#5445=CYLINDRICAL_SURFACE('',#6291,0.25);
#5446=CYLINDRICAL_SURFACE('',#6295,0.33);
#5447=CYLINDRICAL_SURFACE('',#6302,1.51);
#5448=CYLINDRICAL_SURFACE('',#6309,0.25);
#5449=CYLINDRICAL_SURFACE('',#6313,0.33);
#5450=CYLINDRICAL_SURFACE('',#6320,1.51);
#5451=CYLINDRICAL_SURFACE('',#6334,0.57);
#5452=CYLINDRICAL_SURFACE('',#6353,0.19);
#5453=CYLINDRICAL_SURFACE('',#6359,0.19);
#5454=CYLINDRICAL_SURFACE('',#6365,0.19);
#5455=CYLINDRICAL_SURFACE('',#6367,0.125);
#5456=CYLINDRICAL_SURFACE('',#6378,0.685);
#5457=CYLINDRICAL_SURFACE('',#6382,0.165);
#5458=CYLINDRICAL_SURFACE('',#6386,0.165);
#5459=CYLINDRICAL_SURFACE('',#6390,0.275);
#5460=CYLINDRICAL_SURFACE('',#6393,0.275);
#5461=CYLINDRICAL_SURFACE('',#6396,0.275);
#5462=CYLINDRICAL_SURFACE('',#6399,0.275);
#5463=CYLINDRICAL_SURFACE('',#6402,0.7);
#5464=CYLINDRICAL_SURFACE('',#6408,0.93);
#5465=CYLINDRICAL_SURFACE('',#6411,1.3);
#5466=CYLINDRICAL_SURFACE('',#6425,0.165);
#5467=CYLINDRICAL_SURFACE('',#6429,0.165);
#5468=CYLINDRICAL_SURFACE('',#6433,0.275);
#5469=CYLINDRICAL_SURFACE('',#6436,0.275);
#5470=CYLINDRICAL_SURFACE('',#6439,0.275);
#5471=CYLINDRICAL_SURFACE('',#6442,0.275);
#5472=CYLINDRICAL_SURFACE('',#6445,0.7);
#5473=CYLINDRICAL_SURFACE('',#6451,0.93);
#5474=CYLINDRICAL_SURFACE('',#6454,1.3);
#5475=CYLINDRICAL_SURFACE('',#6468,0.275);
#5476=CYLINDRICAL_SURFACE('',#6471,0.275);
#5477=CYLINDRICAL_SURFACE('',#6474,0.275);
#5478=CYLINDRICAL_SURFACE('',#6477,0.275);
#5479=CYLINDRICAL_SURFACE('',#6488,1.6);
#5480=CYLINDRICAL_SURFACE('',#6498,1.2);
#5481=CYLINDRICAL_SURFACE('',#6502,0.405);
#5482=CYLINDRICAL_SURFACE('',#6504,0.7);
#5483=CYLINDRICAL_SURFACE('',#6512,0.61);
#5484=CYLINDRICAL_SURFACE('',#6517,0.405);
#5485=CYLINDRICAL_SURFACE('',#6519,1.);
#5486=CYLINDRICAL_SURFACE('',#6525,0.3);
#5487=CYLINDRICAL_SURFACE('',#6529,0.3);
#5488=CYLINDRICAL_SURFACE('',#6533,0.225);
#5489=CYLINDRICAL_SURFACE('',#6536,0.225);
#5490=CYLINDRICAL_SURFACE('',#6539,0.225);
#5491=CYLINDRICAL_SURFACE('',#6542,0.225);
#5492=CYLINDRICAL_SURFACE('',#6545,1.01);
#5493=CYLINDRICAL_SURFACE('',#6558,0.75);
#5494=CYLINDRICAL_SURFACE('',#6560,1.3);
#5495=CYLINDRICAL_SURFACE('',#6577,0.25);
#5496=CYLINDRICAL_SURFACE('',#6584,0.425);
#5497=CYLINDRICAL_SURFACE('',#6592,0.24505);
#5498=CYLINDRICAL_SURFACE('',#6597,0.265);
#5499=CYLINDRICAL_SURFACE('',#6601,0.5);
#5500=CYLINDRICAL_SURFACE('',#6612,0.2117);
#5501=CYLINDRICAL_SURFACE('',#6631,1.065);
#5502=CYLINDRICAL_SURFACE('',#6637,1.065);
#5503=CYLINDRICAL_SURFACE('',#6643,0.79);
#5504=CYLINDRICAL_SURFACE('',#6645,0.225);
#5505=CYLINDRICAL_SURFACE('',#6648,0.4);
#5506=CYLINDRICAL_SURFACE('',#6658,0.35);
#5507=CYLINDRICAL_SURFACE('',#6666,0.1954);
#5508=CYLINDRICAL_SURFACE('',#6680,0.3);
#5509=CYLINDRICAL_SURFACE('',#6686,0.46);
#5510=CYLINDRICAL_SURFACE('',#6695,0.46);
#5511=CYLINDRICAL_SURFACE('',#6699,0.57);
#5512=CYLINDRICAL_SURFACE('',#6701,0.57);
#5513=CYLINDRICAL_SURFACE('',#6710,0.825);
#5514=CYLINDRICAL_SURFACE('',#6715,1.);
#5515=CYLINDRICAL_SURFACE('',#6721,1.);
#5516=CYLINDRICAL_SURFACE('',#6724,0.825);
#5517=CYLINDRICAL_SURFACE('',#6736,0.685);
#5518=CYLINDRICAL_SURFACE('',#6742,0.685);
#5519=CYLINDRICAL_SURFACE('',#6748,0.46);
#5520=CYLINDRICAL_SURFACE('',#6750,0.2942);
#5521=CYLINDRICAL_SURFACE('',#6825,0.75);
#5522=CYLINDRICAL_SURFACE('',#6831,0.165);
#5523=CYLINDRICAL_SURFACE('',#6862,0.4);
#5524=CYLINDRICAL_SURFACE('',#6877,0.225);
#5525=CYLINDRICAL_SURFACE('',#6880,0.6);
#5526=CYLINDRICAL_SURFACE('',#6907,0.35);
#5527=CYLINDRICAL_SURFACE('',#6915,0.1954);
#5528=ADVANCED_FACE('',(#755),#5431,.F.);
#5529=ADVANCED_FACE('',(#756,#399),#526,.F.);
#5530=ADVANCED_FACE('',(#757),#5432,.F.);
#5531=ADVANCED_FACE('',(#758,#400),#527,.T.);
#5532=ADVANCED_FACE('',(#759),#5433,.F.);
#5533=ADVANCED_FACE('',(#760),#5434,.T.);
#5534=ADVANCED_FACE('',(#761,#401),#528,.T.);
#5535=ADVANCED_FACE('',(#762,#402),#529,.F.);
#5536=ADVANCED_FACE('',(#763),#5435,.F.);
#5537=ADVANCED_FACE('',(#764,#403),#530,.T.);
#5538=ADVANCED_FACE('',(#765),#5436,.F.);
#5539=ADVANCED_FACE('',(#766,#404),#531,.F.);
#5540=ADVANCED_FACE('',(#767),#5437,.F.);
#5541=ADVANCED_FACE('',(#768),#5438,.T.);
#5542=ADVANCED_FACE('',(#769,#405),#532,.T.);
#5543=ADVANCED_FACE('',(#770,#406),#533,.F.);
#5544=ADVANCED_FACE('',(#771),#5439,.F.);
#5545=ADVANCED_FACE('',(#772),#5440,.F.);
#5546=ADVANCED_FACE('',(#773),#5441,.F.);
#5547=ADVANCED_FACE('',(#774),#5442,.F.);
#5548=ADVANCED_FACE('',(#775),#5443,.F.);
#5549=ADVANCED_FACE('',(#776),#5444,.T.);
#5550=ADVANCED_FACE('',(#777,#407),#534,.T.);
#5551=ADVANCED_FACE('',(#778),#5445,.F.);
#5552=ADVANCED_FACE('',(#779),#535,.T.);
#5553=ADVANCED_FACE('',(#780),#5446,.F.);
#5554=ADVANCED_FACE('',(#781,#408),#536,.F.);
#5555=ADVANCED_FACE('',(#782,#409),#537,.F.);
#5556=ADVANCED_FACE('',(#783),#538,.T.);
#5557=ADVANCED_FACE('',(#784),#5447,.F.);
#5558=ADVANCED_FACE('',(#785),#539,.T.);
#5559=ADVANCED_FACE('',(#786),#540,.T.);
#5560=ADVANCED_FACE('',(#787),#541,.T.);
#5561=ADVANCED_FACE('',(#788,#410),#542,.T.);
#5562=ADVANCED_FACE('',(#789),#543,.F.);
#5563=ADVANCED_FACE('',(#790),#5448,.F.);
#5564=ADVANCED_FACE('',(#791),#544,.T.);
#5565=ADVANCED_FACE('',(#792),#5449,.F.);
#5566=ADVANCED_FACE('',(#793,#411),#545,.F.);
#5567=ADVANCED_FACE('',(#794,#412),#546,.F.);
#5568=ADVANCED_FACE('',(#795),#547,.T.);
#5569=ADVANCED_FACE('',(#796),#5450,.F.);
#5570=ADVANCED_FACE('',(#797),#548,.T.);
#5571=ADVANCED_FACE('',(#798),#549,.T.);
#5572=ADVANCED_FACE('',(#799),#550,.T.);
#5573=ADVANCED_FACE('',(#800,#413),#551,.T.);
#5574=ADVANCED_FACE('',(#801),#552,.F.);
#5575=ADVANCED_FACE('',(#802),#553,.T.);
#5576=ADVANCED_FACE('',(#803,#414,#415,#416,#417,#418,#419,#420),#554,.T.);
#5577=ADVANCED_FACE('',(#804),#555,.T.);
#5578=ADVANCED_FACE('',(#805,#421,#422,#423,#424,#425),#556,.T.);
#5579=ADVANCED_FACE('',(#806),#557,.T.);
#5580=ADVANCED_FACE('',(#807),#558,.F.);
#5581=ADVANCED_FACE('',(#808),#5451,.F.);
#5582=ADVANCED_FACE('',(#809),#559,.T.);
#5583=ADVANCED_FACE('',(#810),#560,.T.);
#5584=ADVANCED_FACE('',(#811),#561,.T.);
#5585=ADVANCED_FACE('',(#812),#562,.T.);
#5586=ADVANCED_FACE('',(#813),#563,.T.);
#5587=ADVANCED_FACE('',(#814),#564,.T.);
#5588=ADVANCED_FACE('',(#815,#426),#565,.T.);
#5589=ADVANCED_FACE('',(#816,#427),#566,.F.);
#5590=ADVANCED_FACE('',(#817,#428),#567,.T.);
#5591=ADVANCED_FACE('',(#818),#264,.T.);
#5592=ADVANCED_FACE('',(#819,#429),#568,.T.);
#5593=ADVANCED_FACE('',(#820),#5452,.T.);
#5594=ADVANCED_FACE('',(#821),#265,.T.);
#5595=ADVANCED_FACE('',(#822,#430),#569,.T.);
#5596=ADVANCED_FACE('',(#823),#5453,.T.);
#5597=ADVANCED_FACE('',(#824),#266,.T.);
#5598=ADVANCED_FACE('',(#825,#431),#570,.T.);
#5599=ADVANCED_FACE('',(#826),#5454,.T.);
#5600=ADVANCED_FACE('',(#827),#5455,.F.);
#5601=ADVANCED_FACE('',(#828,#432),#571,.F.);
#5602=ADVANCED_FACE('',(#829),#572,.T.);
#5603=ADVANCED_FACE('',(#830),#573,.T.);
#5604=ADVANCED_FACE('',(#831),#574,.T.);
#5605=ADVANCED_FACE('',(#832),#575,.T.);
#5606=ADVANCED_FACE('',(#833),#576,.T.);
#5607=ADVANCED_FACE('',(#834),#577,.T.);
#5608=ADVANCED_FACE('',(#835,#433),#578,.T.);
#5609=ADVANCED_FACE('',(#836),#5456,.T.);
#5610=ADVANCED_FACE('',(#837,#434),#579,.F.);
#5611=ADVANCED_FACE('',(#838),#5457,.F.);
#5612=ADVANCED_FACE('',(#839),#580,.T.);
#5613=ADVANCED_FACE('',(#840),#5458,.F.);
#5614=ADVANCED_FACE('',(#841),#581,.T.);
#5615=ADVANCED_FACE('',(#842),#5459,.F.);
#5616=ADVANCED_FACE('',(#843),#5460,.F.);
#5617=ADVANCED_FACE('',(#844),#5461,.F.);
#5618=ADVANCED_FACE('',(#845),#5462,.F.);
#5619=ADVANCED_FACE('',(#846),#5463,.F.);
#5620=ADVANCED_FACE('',(#847),#582,.T.);
#5621=ADVANCED_FACE('',(#848,#435,#436),#583,.T.);
#5622=ADVANCED_FACE('',(#849),#5464,.F.);
#5623=ADVANCED_FACE('',(#850),#5465,.F.);
#5624=ADVANCED_FACE('',(#851,#437),#584,.F.);
#5625=ADVANCED_FACE('',(#852,#438),#585,.T.);
#5626=ADVANCED_FACE('',(#853,#439),#258,.F.);
#5627=ADVANCED_FACE('',(#854,#440,#441,#442,#443),#586,.T.);
#5628=ADVANCED_FACE('',(#855),#587,.T.);
#5629=ADVANCED_FACE('',(#856,#444,#445,#446,#447,#448),#588,.T.);
#5630=ADVANCED_FACE('',(#857),#589,.T.);
#5631=ADVANCED_FACE('',(#858),#590,.F.);
#5632=ADVANCED_FACE('',(#859),#5466,.F.);
#5633=ADVANCED_FACE('',(#860),#591,.T.);
#5634=ADVANCED_FACE('',(#861),#5467,.F.);
#5635=ADVANCED_FACE('',(#862),#592,.T.);
#5636=ADVANCED_FACE('',(#863),#5468,.F.);
#5637=ADVANCED_FACE('',(#864),#5469,.F.);
#5638=ADVANCED_FACE('',(#865),#5470,.F.);
#5639=ADVANCED_FACE('',(#866),#5471,.F.);
#5640=ADVANCED_FACE('',(#867),#5472,.F.);
#5641=ADVANCED_FACE('',(#868),#593,.T.);
#5642=ADVANCED_FACE('',(#869,#449,#450),#594,.T.);
#5643=ADVANCED_FACE('',(#870),#5473,.F.);
#5644=ADVANCED_FACE('',(#871),#5474,.F.);
#5645=ADVANCED_FACE('',(#872,#451),#595,.F.);
#5646=ADVANCED_FACE('',(#873,#452),#596,.T.);
#5647=ADVANCED_FACE('',(#874,#453),#259,.F.);
#5648=ADVANCED_FACE('',(#875,#454,#455,#456,#457,#458),#597,.T.);
#5649=ADVANCED_FACE('',(#876),#598,.T.);
#5650=ADVANCED_FACE('',(#877,#459,#460,#461,#462),#599,.T.);
#5651=ADVANCED_FACE('',(#878),#600,.T.);
#5652=ADVANCED_FACE('',(#879),#601,.F.);
#5653=ADVANCED_FACE('',(#880),#5475,.F.);
#5654=ADVANCED_FACE('',(#881),#5476,.F.);
#5655=ADVANCED_FACE('',(#882),#5477,.F.);
#5656=ADVANCED_FACE('',(#883),#5478,.F.);
#5657=ADVANCED_FACE('',(#884),#602,.F.);
#5658=ADVANCED_FACE('',(#885),#603,.F.);
#5659=ADVANCED_FACE('',(#886),#604,.F.);
#5660=ADVANCED_FACE('',(#887),#605,.F.);
#5661=ADVANCED_FACE('',(#888,#463,#464,#465,#466),#606,.T.);
#5662=ADVANCED_FACE('',(#889),#607,.T.);
#5663=ADVANCED_FACE('',(#890),#608,.T.);
#5664=ADVANCED_FACE('',(#891),#5479,.F.);
#5665=ADVANCED_FACE('',(#892),#609,.T.);
#5666=ADVANCED_FACE('',(#893),#610,.T.);
#5667=ADVANCED_FACE('',(#894),#611,.T.);
#5668=ADVANCED_FACE('',(#895,#467,#468,#469,#470),#612,.F.);
#5669=ADVANCED_FACE('',(#896,#471),#613,.F.);
#5670=ADVANCED_FACE('',(#897),#5480,.T.);
#5671=ADVANCED_FACE('',(#898,#472),#614,.T.);
#5672=ADVANCED_FACE('',(#899),#5481,.F.);
#5673=ADVANCED_FACE('',(#900),#5482,.T.);
#5674=ADVANCED_FACE('',(#901,#473),#615,.F.);
#5675=ADVANCED_FACE('',(#902),#257,.T.);
#5676=ADVANCED_FACE('',(#903),#5483,.F.);
#5677=ADVANCED_FACE('',(#904,#474),#616,.F.);
#5678=ADVANCED_FACE('',(#905),#5484,.F.);
#5679=ADVANCED_FACE('',(#906),#5485,.T.);
#5680=ADVANCED_FACE('',(#907,#475),#617,.T.);
#5681=ADVANCED_FACE('',(#908,#476),#618,.F.);
#5682=ADVANCED_FACE('',(#909),#5486,.F.);
#5683=ADVANCED_FACE('',(#910),#619,.T.);
#5684=ADVANCED_FACE('',(#911),#5487,.F.);
#5685=ADVANCED_FACE('',(#912),#620,.T.);
#5686=ADVANCED_FACE('',(#913),#5488,.F.);
#5687=ADVANCED_FACE('',(#914),#5489,.F.);
#5688=ADVANCED_FACE('',(#915),#5490,.F.);
#5689=ADVANCED_FACE('',(#916),#5491,.F.);
#5690=ADVANCED_FACE('',(#917),#5492,.F.);
#5691=ADVANCED_FACE('',(#918),#621,.T.);
#5692=ADVANCED_FACE('',(#919),#622,.T.);
#5693=ADVANCED_FACE('',(#920),#623,.T.);
#5694=ADVANCED_FACE('',(#921),#624,.T.);
#5695=ADVANCED_FACE('',(#922,#477,#478,#479,#480,#481,#482,#483),#625,.T.);
#5696=ADVANCED_FACE('',(#923,#484,#485,#486,#487,#488),#626,.F.);
#5697=ADVANCED_FACE('',(#924,#489),#260,.F.);
#5698=ADVANCED_FACE('',(#925),#5493,.F.);
#5699=ADVANCED_FACE('',(#926),#5494,.T.);
#5700=ADVANCED_FACE('',(#927,#490),#627,.T.);
#5701=ADVANCED_FACE('',(#928,#491),#628,.F.);
#5702=ADVANCED_FACE('',(#929),#629,.F.);
#5703=ADVANCED_FACE('',(#930),#630,.F.);
#5704=ADVANCED_FACE('',(#931),#631,.F.);
#5705=ADVANCED_FACE('',(#932),#632,.F.);
#5706=ADVANCED_FACE('',(#933),#633,.F.);
#5707=ADVANCED_FACE('',(#934),#634,.F.);
#5708=ADVANCED_FACE('',(#935),#635,.F.);
#5709=ADVANCED_FACE('',(#936),#636,.F.);
#5710=ADVANCED_FACE('',(#937,#492),#637,.T.);
#5711=ADVANCED_FACE('',(#938),#5495,.T.);
#5712=ADVANCED_FACE('',(#939),#638,.F.);
#5713=ADVANCED_FACE('',(#940),#639,.T.);
#5714=ADVANCED_FACE('',(#941),#267,.T.);
#5715=ADVANCED_FACE('',(#942),#5496,.T.);
#5716=ADVANCED_FACE('',(#943),#268,.T.);
#5717=ADVANCED_FACE('',(#944,#493),#640,.T.);
#5718=ADVANCED_FACE('',(#945),#269,.T.);
#5719=ADVANCED_FACE('',(#946),#5497,.T.);
#5720=ADVANCED_FACE('',(#947),#270,.F.);
#5721=ADVANCED_FACE('',(#948),#5498,.F.);
#5722=ADVANCED_FACE('',(#949,#494),#641,.T.);
#5723=ADVANCED_FACE('',(#950),#5499,.T.);
#5724=ADVANCED_FACE('',(#951,#495),#642,.F.);
#5725=ADVANCED_FACE('',(#952),#271,.T.);
#5726=ADVANCED_FACE('',(#953),#272,.T.);
#5727=ADVANCED_FACE('',(#954),#643,.T.);
#5728=ADVANCED_FACE('',(#955),#644,.T.);
#5729=ADVANCED_FACE('',(#956),#645,.T.);
#5730=ADVANCED_FACE('',(#957),#5500,.F.);
#5731=ADVANCED_FACE('',(#958),#646,.T.);
#5732=ADVANCED_FACE('',(#959),#647,.T.);
#5733=ADVANCED_FACE('',(#960),#648,.T.);
#5734=ADVANCED_FACE('',(#961,#496),#649,.T.);
#5735=ADVANCED_FACE('',(#962,#497),#650,.F.);
#5736=ADVANCED_FACE('',(#963,#498),#651,.F.);
#5737=ADVANCED_FACE('',(#964,#499),#652,.T.);
#5738=ADVANCED_FACE('',(#965),#653,.T.);
#5739=ADVANCED_FACE('',(#966),#654,.T.);
#5740=ADVANCED_FACE('',(#967),#655,.T.);
#5741=ADVANCED_FACE('',(#968),#656,.T.);
#5742=ADVANCED_FACE('',(#969),#657,.T.);
#5743=ADVANCED_FACE('',(#970),#658,.T.);
#5744=ADVANCED_FACE('',(#971),#5501,.T.);
#5745=ADVANCED_FACE('',(#972,#500),#659,.T.);
#5746=ADVANCED_FACE('',(#973),#273,.T.);
#5747=ADVANCED_FACE('',(#974),#5502,.T.);
#5748=ADVANCED_FACE('',(#975),#274,.T.);
#5749=ADVANCED_FACE('',(#976,#501),#660,.T.);
#5750=ADVANCED_FACE('',(#977),#5503,.F.);
#5751=ADVANCED_FACE('',(#978),#5504,.F.);
#5752=ADVANCED_FACE('',(#979),#5505,.T.);
#5753=ADVANCED_FACE('',(#980,#502),#661,.T.);
#5754=ADVANCED_FACE('',(#981,#503),#662,.F.);
#5755=ADVANCED_FACE('',(#982),#663,.T.);
#5756=ADVANCED_FACE('',(#983),#275,.T.);
#5757=ADVANCED_FACE('',(#984),#5506,.T.);
#5758=ADVANCED_FACE('',(#985),#276,.T.);
#5759=ADVANCED_FACE('',(#986,#504),#664,.T.);
#5760=ADVANCED_FACE('',(#987),#277,.T.);
#5761=ADVANCED_FACE('',(#988),#5507,.T.);
#5762=ADVANCED_FACE('',(#989),#278,.T.);
#5763=ADVANCED_FACE('',(#990),#665,.T.);
#5764=ADVANCED_FACE('',(#991),#666,.F.);
#5765=ADVANCED_FACE('',(#992),#667,.F.);
#5766=ADVANCED_FACE('',(#993),#668,.F.);
#5767=ADVANCED_FACE('',(#994),#669,.F.);
#5768=ADVANCED_FACE('',(#995),#670,.F.);
#5769=ADVANCED_FACE('',(#996),#671,.F.);
#5770=ADVANCED_FACE('',(#997),#672,.F.);
#5771=ADVANCED_FACE('',(#998),#673,.F.);
#5772=ADVANCED_FACE('',(#999),#5508,.T.);
#5773=ADVANCED_FACE('',(#1000),#674,.T.);
#5774=ADVANCED_FACE('',(#1001),#675,.F.);
#5775=ADVANCED_FACE('',(#1002),#5509,.F.);
#5776=ADVANCED_FACE('',(#1003,#505),#261,.F.);
#5777=ADVANCED_FACE('',(#1004),#5510,.F.);
#5778=ADVANCED_FACE('',(#1005,#506),#676,.F.);
#5779=ADVANCED_FACE('',(#1006),#5511,.F.);
#5780=ADVANCED_FACE('',(#1007),#5512,.F.);
#5781=ADVANCED_FACE('',(#1008,#507),#677,.F.);
#5782=ADVANCED_FACE('',(#1009),#262,.T.);
#5783=ADVANCED_FACE('',(#1010),#5513,.T.);
#5784=ADVANCED_FACE('',(#1011,#508),#678,.T.);
#5785=ADVANCED_FACE('',(#1012),#5514,.T.);
#5786=ADVANCED_FACE('',(#1013,#509),#679,.T.);
#5787=ADVANCED_FACE('',(#1014,#510),#680,.T.);
#5788=ADVANCED_FACE('',(#1015),#5515,.T.);
#5789=ADVANCED_FACE('',(#1016,#511),#681,.T.);
#5790=ADVANCED_FACE('',(#1017),#5516,.T.);
#5791=ADVANCED_FACE('',(#1018,#512),#682,.F.);
#5792=ADVANCED_FACE('',(#1019,#513),#683,.T.);
#5793=ADVANCED_FACE('',(#1020),#684,.T.);
#5794=ADVANCED_FACE('',(#1021),#685,.T.);
#5795=ADVANCED_FACE('',(#1022),#686,.T.);
#5796=ADVANCED_FACE('',(#1023),#687,.T.);
#5797=ADVANCED_FACE('',(#1024),#688,.T.);
#5798=ADVANCED_FACE('',(#1025),#689,.T.);
#5799=ADVANCED_FACE('',(#1026),#5517,.T.);
#5800=ADVANCED_FACE('',(#1027,#514),#690,.T.);
#5801=ADVANCED_FACE('',(#1028),#279,.T.);
#5802=ADVANCED_FACE('',(#1029),#5518,.T.);
#5803=ADVANCED_FACE('',(#1030),#280,.T.);
#5804=ADVANCED_FACE('',(#1031,#515),#691,.T.);
#5805=ADVANCED_FACE('',(#1032),#5519,.F.);
#5806=ADVANCED_FACE('',(#1033),#5520,.T.);
#5807=ADVANCED_FACE('',(#1034),#281,.T.);
#5808=ADVANCED_FACE('',(#1035),#692,.T.);
#5809=ADVANCED_FACE('',(#1036),#282,.T.);
#5810=ADVANCED_FACE('',(#1037),#693,.T.);
#5811=ADVANCED_FACE('',(#1038),#694,.T.);
#5812=ADVANCED_FACE('',(#1039),#695,.T.);
#5813=ADVANCED_FACE('',(#1040),#696,.T.);
#5814=ADVANCED_FACE('',(#1041),#697,.T.);
#5815=ADVANCED_FACE('',(#1042),#698,.T.);
#5816=ADVANCED_FACE('',(#1043),#699,.T.);
#5817=ADVANCED_FACE('',(#1044,#516),#700,.F.);
#5818=ADVANCED_FACE('',(#1045),#701,.F.);
#5819=ADVANCED_FACE('',(#1046),#702,.F.);
#5820=ADVANCED_FACE('',(#1047),#703,.F.);
#5821=ADVANCED_FACE('',(#1048),#704,.F.);
#5822=ADVANCED_FACE('',(#1049),#705,.T.);
#5823=ADVANCED_FACE('',(#1050),#5521,.F.);
#5824=ADVANCED_FACE('',(#1051,#517,#518),#263,.T.);
#5825=ADVANCED_FACE('',(#1052),#5522,.F.);
#5826=ADVANCED_FACE('',(#1053),#706,.T.);
#5827=ADVANCED_FACE('',(#1054),#707,.F.);
#5828=ADVANCED_FACE('',(#1055),#708,.F.);
#5829=ADVANCED_FACE('',(#1056),#709,.F.);
#5830=ADVANCED_FACE('',(#1057),#710,.F.);
#5831=ADVANCED_FACE('',(#1058),#711,.T.);
#5832=ADVANCED_FACE('',(#1059),#712,.T.);
#5833=ADVANCED_FACE('',(#1060),#713,.T.);
#5834=ADVANCED_FACE('',(#1061),#714,.T.);
#5835=ADVANCED_FACE('',(#1062,#519),#715,.T.);
#5836=ADVANCED_FACE('',(#1063),#716,.T.);
#5837=ADVANCED_FACE('',(#1064),#717,.T.);
#5838=ADVANCED_FACE('',(#1065),#718,.T.);
#5839=ADVANCED_FACE('',(#1066),#719,.T.);
#5840=ADVANCED_FACE('',(#1067),#720,.T.);
#5841=ADVANCED_FACE('',(#1068),#721,.T.);
#5842=ADVANCED_FACE('',(#1069),#722,.T.);
#5843=ADVANCED_FACE('',(#1070),#723,.T.);
#5844=ADVANCED_FACE('',(#1071),#724,.F.);
#5845=ADVANCED_FACE('',(#1072),#5523,.T.);
#5846=ADVANCED_FACE('',(#1073,#520),#725,.F.);
#5847=ADVANCED_FACE('',(#1074),#726,.F.);
#5848=ADVANCED_FACE('',(#1075),#727,.F.);
#5849=ADVANCED_FACE('',(#1076),#728,.F.);
#5850=ADVANCED_FACE('',(#1077),#729,.F.);
#5851=ADVANCED_FACE('',(#1078),#730,.T.);
#5852=ADVANCED_FACE('',(#1079),#731,.T.);
#5853=ADVANCED_FACE('',(#1080),#732,.T.);
#5854=ADVANCED_FACE('',(#1081),#733,.T.);
#5855=ADVANCED_FACE('',(#1082,#521),#734,.T.);
#5856=ADVANCED_FACE('',(#1083,#522),#735,.F.);
#5857=ADVANCED_FACE('',(#1084),#5524,.F.);
#5858=ADVANCED_FACE('',(#1085),#5525,.T.);
#5859=ADVANCED_FACE('',(#1086,#523),#736,.T.);
#5860=ADVANCED_FACE('',(#1087,#524),#737,.F.);
#5861=ADVANCED_FACE('',(#1088),#738,.T.);
#5862=ADVANCED_FACE('',(#1089),#739,.T.);
#5863=ADVANCED_FACE('',(#1090),#740,.T.);
#5864=ADVANCED_FACE('',(#1091),#741,.T.);
#5865=ADVANCED_FACE('',(#1092),#742,.T.);
#5866=ADVANCED_FACE('',(#1093),#743,.F.);
#5867=ADVANCED_FACE('',(#1094),#744,.F.);
#5868=ADVANCED_FACE('',(#1095),#745,.F.);
#5869=ADVANCED_FACE('',(#1096),#746,.F.);
#5870=ADVANCED_FACE('',(#1097),#747,.F.);
#5871=ADVANCED_FACE('',(#1098),#748,.F.);
#5872=ADVANCED_FACE('',(#1099),#749,.F.);
#5873=ADVANCED_FACE('',(#1100),#750,.F.);
#5874=ADVANCED_FACE('',(#1101),#751,.F.);
#5875=ADVANCED_FACE('',(#1102),#752,.F.);
#5876=ADVANCED_FACE('',(#1103),#753,.T.);
#5877=ADVANCED_FACE('',(#1104),#283,.T.);
#5878=ADVANCED_FACE('',(#1105),#5526,.T.);
#5879=ADVANCED_FACE('',(#1106),#284,.T.);
#5880=ADVANCED_FACE('',(#1107,#525),#754,.T.);
#5881=ADVANCED_FACE('',(#1108),#285,.T.);
#5882=ADVANCED_FACE('',(#1109),#5527,.T.);
#5883=CLOSED_SHELL('',(#5528,#5529,#5530,#5531,#5532,#5533,#5534,#5535));
#5884=CLOSED_SHELL('',(#5536,#5537,#5538,#5539,#5540,#5541,#5542,#5543));
#5885=CLOSED_SHELL('',(#5544,#5545,#5546,#5547,#5548,#5549,#5550,#5551,
#5552,#5553,#5554,#5555,#5556,#5557,#5558,#5559,#5560,#5561,#5562,#5563,
#5564,#5565,#5566,#5567,#5568,#5569,#5570,#5571,#5572,#5573,#5574,#5575,
#5576,#5577,#5578,#5579,#5580));
#5886=CLOSED_SHELL('',(#5581,#5582,#5583,#5584,#5585,#5586,#5587,#5588,
#5589));
#5887=CLOSED_SHELL('',(#5590,#5591,#5592,#5593,#5594,#5595,#5596,#5597,
#5598,#5599,#5600,#5601,#5602,#5603,#5604,#5605,#5606,#5607,#5608,#5609,
#5610));
#5888=CLOSED_SHELL('',(#5611,#5612,#5613,#5614,#5615,#5616,#5617,#5618,
#5619,#5620,#5621,#5622,#5623,#5624,#5625,#5626,#5627,#5628,#5629,#5630,
#5631));
#5889=CLOSED_SHELL('',(#5632,#5633,#5634,#5635,#5636,#5637,#5638,#5639,
#5640,#5641,#5642,#5643,#5644,#5645,#5646,#5647,#5648,#5649,#5650,#5651,
#5652));
#5890=CLOSED_SHELL('',(#5653,#5654,#5655,#5656,#5657,#5658,#5659,#5660,
#5661,#5662,#5663,#5664,#5665,#5666,#5667,#5668));
#5891=CLOSED_SHELL('',(#5669,#5670,#5671,#5672,#5673,#5674));
#5892=CLOSED_SHELL('',(#5675));
#5893=CLOSED_SHELL('',(#5676,#5677,#5678,#5679,#5680,#5681));
#5894=CLOSED_SHELL('',(#5682,#5683,#5684,#5685,#5686,#5687,#5688,#5689,
#5690,#5691,#5692,#5693,#5694,#5695,#5696));
#5895=CLOSED_SHELL('',(#5697,#5698,#5699,#5700,#5701));
#5896=CLOSED_SHELL('',(#5702,#5703,#5704,#5705,#5706,#5707,#5708,#5709));
#5897=CLOSED_SHELL('',(#5710,#5711,#5712,#5713,#5714,#5715,#5716,#5717,
#5718,#5719));
#5898=CLOSED_SHELL('',(#5720,#5721,#5722,#5723,#5724));
#5899=CLOSED_SHELL('',(#5725,#5726,#5727,#5728,#5729,#5730,#5731,#5732,
#5733,#5734,#5735));
#5900=CLOSED_SHELL('',(#5736,#5737,#5738,#5739,#5740,#5741,#5742,#5743,
#5744,#5745,#5746,#5747,#5748,#5749,#5750));
#5901=CLOSED_SHELL('',(#5751,#5752,#5753,#5754));
#5902=CLOSED_SHELL('',(#5755,#5756,#5757,#5758,#5759,#5760,#5761,#5762,
#5763));
#5903=CLOSED_SHELL('',(#5764,#5765,#5766,#5767,#5768,#5769,#5770,#5771));
#5904=CLOSED_SHELL('',(#5772,#5773,#5774));
#5905=CLOSED_SHELL('',(#5775,#5776,#5777,#5778,#5779,#5780,#5781,#5782,
#5783,#5784,#5785,#5786,#5787,#5788,#5789,#5790));
#5906=CLOSED_SHELL('',(#5791,#5792,#5793,#5794,#5795,#5796,#5797,#5798,
#5799,#5800,#5801,#5802,#5803,#5804,#5805));
#5907=CLOSED_SHELL('',(#5806,#5807,#5808,#5809,#5810,#5811,#5812,#5813,
#5814,#5815,#5816,#5817));
#5908=CLOSED_SHELL('',(#5818,#5819,#5820,#5821,#5822,#5823,#5824));
#5909=CLOSED_SHELL('',(#5825,#5826,#5827,#5828,#5829,#5830,#5831,#5832,
#5833,#5834,#5835,#5836,#5837,#5838,#5839,#5840,#5841,#5842,#5843,#5844,
#5845,#5846));
#5910=CLOSED_SHELL('',(#5847,#5848,#5849,#5850,#5851,#5852,#5853,#5854,
#5855,#5856));
#5911=CLOSED_SHELL('',(#5857,#5858,#5859,#5860));
#5912=CLOSED_SHELL('',(#5861,#5862,#5863,#5864,#5865,#5866));
#5913=CLOSED_SHELL('',(#5867,#5868,#5869,#5870,#5871,#5872,#5873,#5874));
#5914=CLOSED_SHELL('',(#5875,#5876,#5877,#5878,#5879,#5880,#5881,#5882));
#5915=DERIVED_UNIT_ELEMENT(#5973,1.);
#5916=DERIVED_UNIT_ELEMENT(#10519,-3.);
#5917=DERIVED_UNIT_ELEMENT(#5973,1.);
#5918=DERIVED_UNIT_ELEMENT(#10519,-3.);
#5919=DERIVED_UNIT_ELEMENT(#5973,1.);
#5920=DERIVED_UNIT_ELEMENT(#10519,-3.);
#5921=DERIVED_UNIT_ELEMENT(#5973,1.);
#5922=DERIVED_UNIT_ELEMENT(#10519,-3.);
#5923=DERIVED_UNIT_ELEMENT(#5973,1.);
#5924=DERIVED_UNIT_ELEMENT(#10519,-3.);
#5925=DERIVED_UNIT_ELEMENT(#5973,1.);
#5926=DERIVED_UNIT_ELEMENT(#10519,-3.);
#5927=DERIVED_UNIT_ELEMENT(#5973,1.);
#5928=DERIVED_UNIT_ELEMENT(#10519,-3.);
#5929=DERIVED_UNIT_ELEMENT(#5973,1.);
#5930=DERIVED_UNIT_ELEMENT(#10519,-3.);
#5931=DERIVED_UNIT_ELEMENT(#5973,1.);
#5932=DERIVED_UNIT_ELEMENT(#10519,-3.);
#5933=DERIVED_UNIT_ELEMENT(#5973,1.);
#5934=DERIVED_UNIT_ELEMENT(#10519,-3.);
#5935=DERIVED_UNIT_ELEMENT(#5973,1.);
#5936=DERIVED_UNIT_ELEMENT(#10519,-3.);
#5937=DERIVED_UNIT_ELEMENT(#5973,1.);
#5938=DERIVED_UNIT_ELEMENT(#10519,-3.);
#5939=DERIVED_UNIT_ELEMENT(#5973,1.);
#5940=DERIVED_UNIT_ELEMENT(#10519,-3.);
#5941=DERIVED_UNIT_ELEMENT(#5973,1.);
#5942=DERIVED_UNIT_ELEMENT(#10519,-3.);
#5943=DERIVED_UNIT_ELEMENT(#5973,1.);
#5944=DERIVED_UNIT_ELEMENT(#10519,-3.);
#5945=DERIVED_UNIT_ELEMENT(#5973,1.);
#5946=DERIVED_UNIT_ELEMENT(#10519,-3.);
#5947=DERIVED_UNIT_ELEMENT(#5973,1.);
#5948=DERIVED_UNIT_ELEMENT(#10519,-3.);
#5949=DERIVED_UNIT_ELEMENT(#5973,1.);
#5950=DERIVED_UNIT_ELEMENT(#10519,-3.);
#5951=DERIVED_UNIT_ELEMENT(#5973,1.);
#5952=DERIVED_UNIT_ELEMENT(#10519,-3.);
#5953=DERIVED_UNIT_ELEMENT(#5973,1.);
#5954=DERIVED_UNIT_ELEMENT(#10519,-3.);
#5955=DERIVED_UNIT_ELEMENT(#5973,1.);
#5956=DERIVED_UNIT_ELEMENT(#10519,-3.);
#5957=DERIVED_UNIT_ELEMENT(#5973,1.);
#5958=DERIVED_UNIT_ELEMENT(#10519,-3.);
#5959=DERIVED_UNIT_ELEMENT(#5973,1.);
#5960=DERIVED_UNIT_ELEMENT(#10519,-3.);
#5961=DERIVED_UNIT_ELEMENT(#5973,1.);
#5962=DERIVED_UNIT_ELEMENT(#10519,-3.);
#5963=DERIVED_UNIT_ELEMENT(#5973,1.);
#5964=DERIVED_UNIT_ELEMENT(#10519,-3.);
#5965=DERIVED_UNIT_ELEMENT(#5973,1.);
#5966=DERIVED_UNIT_ELEMENT(#10519,-3.);
#5967=DERIVED_UNIT_ELEMENT(#5973,1.);
#5968=DERIVED_UNIT_ELEMENT(#10519,-3.);
#5969=DERIVED_UNIT_ELEMENT(#5973,1.);
#5970=DERIVED_UNIT_ELEMENT(#10519,-3.);
#5971=DERIVED_UNIT_ELEMENT(#5973,1.);
#5972=DERIVED_UNIT_ELEMENT(#10519,-3.);
#5973=(
MASS_UNIT()
NAMED_UNIT(*)
SI_UNIT(.KILO.,.GRAM.)
);
#5974=DERIVED_UNIT((#5915,#5916));
#5975=DERIVED_UNIT((#5917,#5918));
#5976=DERIVED_UNIT((#5919,#5920));
#5977=DERIVED_UNIT((#5921,#5922));
#5978=DERIVED_UNIT((#5923,#5924));
#5979=DERIVED_UNIT((#5925,#5926));
#5980=DERIVED_UNIT((#5927,#5928));
#5981=DERIVED_UNIT((#5929,#5930));
#5982=DERIVED_UNIT((#5931,#5932));
#5983=DERIVED_UNIT((#5933,#5934));
#5984=DERIVED_UNIT((#5935,#5936));
#5985=DERIVED_UNIT((#5937,#5938));
#5986=DERIVED_UNIT((#5939,#5940));
#5987=DERIVED_UNIT((#5941,#5942));
#5988=DERIVED_UNIT((#5943,#5944));
#5989=DERIVED_UNIT((#5945,#5946));
#5990=DERIVED_UNIT((#5947,#5948));
#5991=DERIVED_UNIT((#5949,#5950));
#5992=DERIVED_UNIT((#5951,#5952));
#5993=DERIVED_UNIT((#5953,#5954));
#5994=DERIVED_UNIT((#5955,#5956));
#5995=DERIVED_UNIT((#5957,#5958));
#5996=DERIVED_UNIT((#5959,#5960));
#5997=DERIVED_UNIT((#5961,#5962));
#5998=DERIVED_UNIT((#5963,#5964));
#5999=DERIVED_UNIT((#5965,#5966));
#6000=DERIVED_UNIT((#5967,#5968));
#6001=DERIVED_UNIT((#5969,#5970));
#6002=DERIVED_UNIT((#5971,#5972));
#6003=MEASURE_REPRESENTATION_ITEM('density measure',
POSITIVE_RATIO_MEASURE(7850.),#5974);
#6004=MEASURE_REPRESENTATION_ITEM('density measure',
POSITIVE_RATIO_MEASURE(7850.),#5975);
#6005=MEASURE_REPRESENTATION_ITEM('density measure',
POSITIVE_RATIO_MEASURE(7850.),#5976);
#6006=MEASURE_REPRESENTATION_ITEM('density measure',
POSITIVE_RATIO_MEASURE(7850.),#5977);
#6007=MEASURE_REPRESENTATION_ITEM('density measure',
POSITIVE_RATIO_MEASURE(7850.),#5978);
#6008=MEASURE_REPRESENTATION_ITEM('density measure',
POSITIVE_RATIO_MEASURE(7850.),#5979);
#6009=MEASURE_REPRESENTATION_ITEM('density measure',
POSITIVE_RATIO_MEASURE(7850.),#5980);
#6010=MEASURE_REPRESENTATION_ITEM('density measure',
POSITIVE_RATIO_MEASURE(7850.),#5981);
#6011=MEASURE_REPRESENTATION_ITEM('density measure',
POSITIVE_RATIO_MEASURE(7850.),#5982);
#6012=MEASURE_REPRESENTATION_ITEM('density measure',
POSITIVE_RATIO_MEASURE(7850.),#5983);
#6013=MEASURE_REPRESENTATION_ITEM('density measure',
POSITIVE_RATIO_MEASURE(7850.),#5984);
#6014=MEASURE_REPRESENTATION_ITEM('density measure',
POSITIVE_RATIO_MEASURE(7850.),#5985);
#6015=MEASURE_REPRESENTATION_ITEM('density measure',
POSITIVE_RATIO_MEASURE(7850.),#5986);
#6016=MEASURE_REPRESENTATION_ITEM('density measure',
POSITIVE_RATIO_MEASURE(7850.),#5987);
#6017=MEASURE_REPRESENTATION_ITEM('density measure',
POSITIVE_RATIO_MEASURE(7850.),#5988);
#6018=MEASURE_REPRESENTATION_ITEM('density measure',
POSITIVE_RATIO_MEASURE(7850.),#5989);
#6019=MEASURE_REPRESENTATION_ITEM('density measure',
POSITIVE_RATIO_MEASURE(7850.),#5990);
#6020=MEASURE_REPRESENTATION_ITEM('density measure',
POSITIVE_RATIO_MEASURE(7850.),#5991);
#6021=MEASURE_REPRESENTATION_ITEM('density measure',
POSITIVE_RATIO_MEASURE(7850.),#5992);
#6022=MEASURE_REPRESENTATION_ITEM('density measure',
POSITIVE_RATIO_MEASURE(7850.),#5993);
#6023=MEASURE_REPRESENTATION_ITEM('density measure',
POSITIVE_RATIO_MEASURE(7850.),#5994);
#6024=MEASURE_REPRESENTATION_ITEM('density measure',
POSITIVE_RATIO_MEASURE(7850.),#5995);
#6025=MEASURE_REPRESENTATION_ITEM('density measure',
POSITIVE_RATIO_MEASURE(7850.),#5996);
#6026=MEASURE_REPRESENTATION_ITEM('density measure',
POSITIVE_RATIO_MEASURE(7850.),#5997);
#6027=MEASURE_REPRESENTATION_ITEM('density measure',
POSITIVE_RATIO_MEASURE(7850.),#5998);
#6028=MEASURE_REPRESENTATION_ITEM('density measure',
POSITIVE_RATIO_MEASURE(7850.),#5999);
#6029=MEASURE_REPRESENTATION_ITEM('density measure',
POSITIVE_RATIO_MEASURE(7850.),#6000);
#6030=MEASURE_REPRESENTATION_ITEM('density measure',
POSITIVE_RATIO_MEASURE(7850.),#6001);
#6031=MEASURE_REPRESENTATION_ITEM('density measure',
POSITIVE_RATIO_MEASURE(7850.),#6002);
#6032=PROPERTY_DEFINITION_REPRESENTATION(#6177,#6090);
#6033=PROPERTY_DEFINITION_REPRESENTATION(#6178,#6091);
#6034=PROPERTY_DEFINITION_REPRESENTATION(#6179,#6092);
#6035=PROPERTY_DEFINITION_REPRESENTATION(#6180,#6093);
#6036=PROPERTY_DEFINITION_REPRESENTATION(#6181,#6094);
#6037=PROPERTY_DEFINITION_REPRESENTATION(#6182,#6095);
#6038=PROPERTY_DEFINITION_REPRESENTATION(#6183,#6096);
#6039=PROPERTY_DEFINITION_REPRESENTATION(#6184,#6097);
#6040=PROPERTY_DEFINITION_REPRESENTATION(#6185,#6098);
#6041=PROPERTY_DEFINITION_REPRESENTATION(#6186,#6099);
#6042=PROPERTY_DEFINITION_REPRESENTATION(#6187,#6100);
#6043=PROPERTY_DEFINITION_REPRESENTATION(#6188,#6101);
#6044=PROPERTY_DEFINITION_REPRESENTATION(#6189,#6102);
#6045=PROPERTY_DEFINITION_REPRESENTATION(#6190,#6103);
#6046=PROPERTY_DEFINITION_REPRESENTATION(#6191,#6104);
#6047=PROPERTY_DEFINITION_REPRESENTATION(#6192,#6105);
#6048=PROPERTY_DEFINITION_REPRESENTATION(#6193,#6106);
#6049=PROPERTY_DEFINITION_REPRESENTATION(#6194,#6107);
#6050=PROPERTY_DEFINITION_REPRESENTATION(#6195,#6108);
#6051=PROPERTY_DEFINITION_REPRESENTATION(#6196,#6109);
#6052=PROPERTY_DEFINITION_REPRESENTATION(#6197,#6110);
#6053=PROPERTY_DEFINITION_REPRESENTATION(#6198,#6111);
#6054=PROPERTY_DEFINITION_REPRESENTATION(#6199,#6112);
#6055=PROPERTY_DEFINITION_REPRESENTATION(#6200,#6113);
#6056=PROPERTY_DEFINITION_REPRESENTATION(#6201,#6114);
#6057=PROPERTY_DEFINITION_REPRESENTATION(#6202,#6115);
#6058=PROPERTY_DEFINITION_REPRESENTATION(#6203,#6116);
#6059=PROPERTY_DEFINITION_REPRESENTATION(#6204,#6117);
#6060=PROPERTY_DEFINITION_REPRESENTATION(#6205,#6118);
#6061=PROPERTY_DEFINITION_REPRESENTATION(#6206,#6119);
#6062=PROPERTY_DEFINITION_REPRESENTATION(#6207,#6120);
#6063=PROPERTY_DEFINITION_REPRESENTATION(#6208,#6121);
#6064=PROPERTY_DEFINITION_REPRESENTATION(#6209,#6122);
#6065=PROPERTY_DEFINITION_REPRESENTATION(#6210,#6123);
#6066=PROPERTY_DEFINITION_REPRESENTATION(#6211,#6124);
#6067=PROPERTY_DEFINITION_REPRESENTATION(#6212,#6125);
#6068=PROPERTY_DEFINITION_REPRESENTATION(#6213,#6126);
#6069=PROPERTY_DEFINITION_REPRESENTATION(#6214,#6127);
#6070=PROPERTY_DEFINITION_REPRESENTATION(#6215,#6128);
#6071=PROPERTY_DEFINITION_REPRESENTATION(#6216,#6129);
#6072=PROPERTY_DEFINITION_REPRESENTATION(#6217,#6130);
#6073=PROPERTY_DEFINITION_REPRESENTATION(#6218,#6131);
#6074=PROPERTY_DEFINITION_REPRESENTATION(#6219,#6132);
#6075=PROPERTY_DEFINITION_REPRESENTATION(#6220,#6133);
#6076=PROPERTY_DEFINITION_REPRESENTATION(#6221,#6134);
#6077=PROPERTY_DEFINITION_REPRESENTATION(#6222,#6135);
#6078=PROPERTY_DEFINITION_REPRESENTATION(#6223,#6136);
#6079=PROPERTY_DEFINITION_REPRESENTATION(#6224,#6137);
#6080=PROPERTY_DEFINITION_REPRESENTATION(#6225,#6138);
#6081=PROPERTY_DEFINITION_REPRESENTATION(#6226,#6139);
#6082=PROPERTY_DEFINITION_REPRESENTATION(#6227,#6140);
#6083=PROPERTY_DEFINITION_REPRESENTATION(#6228,#6141);
#6084=PROPERTY_DEFINITION_REPRESENTATION(#6229,#6142);
#6085=PROPERTY_DEFINITION_REPRESENTATION(#6230,#6143);
#6086=PROPERTY_DEFINITION_REPRESENTATION(#6231,#6144);
#6087=PROPERTY_DEFINITION_REPRESENTATION(#6232,#6145);
#6088=PROPERTY_DEFINITION_REPRESENTATION(#6233,#6146);
#6089=PROPERTY_DEFINITION_REPRESENTATION(#6234,#6147);
#6090=REPRESENTATION('material name',(#6148),#10487);
#6091=REPRESENTATION('density',(#6003),#10487);
#6092=REPRESENTATION('material name',(#6149),#10488);
#6093=REPRESENTATION('density',(#6004),#10488);
#6094=REPRESENTATION('material name',(#6150),#10489);
#6095=REPRESENTATION('density',(#6005),#10489);
#6096=REPRESENTATION('material name',(#6151),#10490);
#6097=REPRESENTATION('density',(#6006),#10490);
#6098=REPRESENTATION('material name',(#6152),#10491);
#6099=REPRESENTATION('density',(#6007),#10491);
#6100=REPRESENTATION('material name',(#6153),#10492);
#6101=REPRESENTATION('density',(#6008),#10492);
#6102=REPRESENTATION('material name',(#6154),#10493);
#6103=REPRESENTATION('density',(#6009),#10493);
#6104=REPRESENTATION('material name',(#6155),#10494);
#6105=REPRESENTATION('density',(#6010),#10494);
#6106=REPRESENTATION('material name',(#6156),#10495);
#6107=REPRESENTATION('density',(#6011),#10495);
#6108=REPRESENTATION('material name',(#6157),#10496);
#6109=REPRESENTATION('density',(#6012),#10496);
#6110=REPRESENTATION('material name',(#6158),#10497);
#6111=REPRESENTATION('density',(#6013),#10497);
#6112=REPRESENTATION('material name',(#6159),#10498);
#6113=REPRESENTATION('density',(#6014),#10498);
#6114=REPRESENTATION('material name',(#6160),#10499);
#6115=REPRESENTATION('density',(#6015),#10499);
#6116=REPRESENTATION('material name',(#6161),#10500);
#6117=REPRESENTATION('density',(#6016),#10500);
#6118=REPRESENTATION('material name',(#6162),#10501);
#6119=REPRESENTATION('density',(#6017),#10501);
#6120=REPRESENTATION('material name',(#6163),#10502);
#6121=REPRESENTATION('density',(#6018),#10502);
#6122=REPRESENTATION('material name',(#6164),#10503);
#6123=REPRESENTATION('density',(#6019),#10503);
#6124=REPRESENTATION('material name',(#6165),#10504);
#6125=REPRESENTATION('density',(#6020),#10504);
#6126=REPRESENTATION('material name',(#6166),#10505);
#6127=REPRESENTATION('density',(#6021),#10505);
#6128=REPRESENTATION('material name',(#6167),#10506);
#6129=REPRESENTATION('density',(#6022),#10506);
#6130=REPRESENTATION('material name',(#6168),#10507);
#6131=REPRESENTATION('density',(#6023),#10507);
#6132=REPRESENTATION('material name',(#6169),#10508);
#6133=REPRESENTATION('density',(#6024),#10508);
#6134=REPRESENTATION('material name',(#6170),#10509);
#6135=REPRESENTATION('density',(#6025),#10509);
#6136=REPRESENTATION('material name',(#6171),#10511);
#6137=REPRESENTATION('density',(#6026),#10511);
#6138=REPRESENTATION('material name',(#6172),#10512);
#6139=REPRESENTATION('density',(#6027),#10512);
#6140=REPRESENTATION('material name',(#6173),#10513);
#6141=REPRESENTATION('density',(#6028),#10513);
#6142=REPRESENTATION('material name',(#6174),#10514);
#6143=REPRESENTATION('density',(#6029),#10514);
#6144=REPRESENTATION('material name',(#6175),#10515);
#6145=REPRESENTATION('density',(#6030),#10515);
#6146=REPRESENTATION('material name',(#6176),#10516);
#6147=REPRESENTATION('density',(#6031),#10516);
#6148=DESCRIPTIVE_REPRESENTATION_ITEM('Steel','Steel');
#6149=DESCRIPTIVE_REPRESENTATION_ITEM('Steel','Steel');
#6150=DESCRIPTIVE_REPRESENTATION_ITEM('Steel','Steel');
#6151=DESCRIPTIVE_REPRESENTATION_ITEM('Steel','Steel');
#6152=DESCRIPTIVE_REPRESENTATION_ITEM('Steel','Steel');
#6153=DESCRIPTIVE_REPRESENTATION_ITEM('Steel','Steel');
#6154=DESCRIPTIVE_REPRESENTATION_ITEM('Steel','Steel');
#6155=DESCRIPTIVE_REPRESENTATION_ITEM('Steel','Steel');
#6156=DESCRIPTIVE_REPRESENTATION_ITEM('Steel','Steel');
#6157=DESCRIPTIVE_REPRESENTATION_ITEM('Steel','Steel');
#6158=DESCRIPTIVE_REPRESENTATION_ITEM('Steel','Steel');
#6159=DESCRIPTIVE_REPRESENTATION_ITEM('Steel','Steel');
#6160=DESCRIPTIVE_REPRESENTATION_ITEM('Steel','Steel');
#6161=DESCRIPTIVE_REPRESENTATION_ITEM('Steel','Steel');
#6162=DESCRIPTIVE_REPRESENTATION_ITEM('Steel','Steel');
#6163=DESCRIPTIVE_REPRESENTATION_ITEM('Steel','Steel');
#6164=DESCRIPTIVE_REPRESENTATION_ITEM('Steel','Steel');
#6165=DESCRIPTIVE_REPRESENTATION_ITEM('Steel','Steel');
#6166=DESCRIPTIVE_REPRESENTATION_ITEM('Steel','Steel');
#6167=DESCRIPTIVE_REPRESENTATION_ITEM('Steel','Steel');
#6168=DESCRIPTIVE_REPRESENTATION_ITEM('Steel','Steel');
#6169=DESCRIPTIVE_REPRESENTATION_ITEM('Steel','Steel');
#6170=DESCRIPTIVE_REPRESENTATION_ITEM('Steel','Steel');
#6171=DESCRIPTIVE_REPRESENTATION_ITEM('Steel','Steel');
#6172=DESCRIPTIVE_REPRESENTATION_ITEM('Steel','Steel');
#6173=DESCRIPTIVE_REPRESENTATION_ITEM('Steel','Steel');
#6174=DESCRIPTIVE_REPRESENTATION_ITEM('Steel','Steel');
#6175=DESCRIPTIVE_REPRESENTATION_ITEM('Steel','Steel');
#6176=DESCRIPTIVE_REPRESENTATION_ITEM('Steel','Steel');
#6177=PROPERTY_DEFINITION('material property','material name',#10676);
#6178=PROPERTY_DEFINITION('material property','density of part',#10676);
#6179=PROPERTY_DEFINITION('material property','material name',#10677);
#6180=PROPERTY_DEFINITION('material property','density of part',#10677);
#6181=PROPERTY_DEFINITION('material property','material name',#10678);
#6182=PROPERTY_DEFINITION('material property','density of part',#10678);
#6183=PROPERTY_DEFINITION('material property','material name',#10679);
#6184=PROPERTY_DEFINITION('material property','density of part',#10679);
#6185=PROPERTY_DEFINITION('material property','material name',#10680);
#6186=PROPERTY_DEFINITION('material property','density of part',#10680);
#6187=PROPERTY_DEFINITION('material property','material name',#10681);
#6188=PROPERTY_DEFINITION('material property','density of part',#10681);
#6189=PROPERTY_DEFINITION('material property','material name',#10682);
#6190=PROPERTY_DEFINITION('material property','density of part',#10682);
#6191=PROPERTY_DEFINITION('material property','material name',#10683);
#6192=PROPERTY_DEFINITION('material property','density of part',#10683);
#6193=PROPERTY_DEFINITION('material property','material name',#10684);
#6194=PROPERTY_DEFINITION('material property','density of part',#10684);
#6195=PROPERTY_DEFINITION('material property','material name',#10685);
#6196=PROPERTY_DEFINITION('material property','density of part',#10685);
#6197=PROPERTY_DEFINITION('material property','material name',#10686);
#6198=PROPERTY_DEFINITION('material property','density of part',#10686);
#6199=PROPERTY_DEFINITION('material property','material name',#10687);
#6200=PROPERTY_DEFINITION('material property','density of part',#10687);
#6201=PROPERTY_DEFINITION('material property','material name',#10688);
#6202=PROPERTY_DEFINITION('material property','density of part',#10688);
#6203=PROPERTY_DEFINITION('material property','material name',#10689);
#6204=PROPERTY_DEFINITION('material property','density of part',#10689);
#6205=PROPERTY_DEFINITION('material property','material name',#10690);
#6206=PROPERTY_DEFINITION('material property','density of part',#10690);
#6207=PROPERTY_DEFINITION('material property','material name',#10691);
#6208=PROPERTY_DEFINITION('material property','density of part',#10691);
#6209=PROPERTY_DEFINITION('material property','material name',#10692);
#6210=PROPERTY_DEFINITION('material property','density of part',#10692);
#6211=PROPERTY_DEFINITION('material property','material name',#10693);
#6212=PROPERTY_DEFINITION('material property','density of part',#10693);
#6213=PROPERTY_DEFINITION('material property','material name',#10694);
#6214=PROPERTY_DEFINITION('material property','density of part',#10694);
#6215=PROPERTY_DEFINITION('material property','material name',#10695);
#6216=PROPERTY_DEFINITION('material property','density of part',#10695);
#6217=PROPERTY_DEFINITION('material property','material name',#10696);
#6218=PROPERTY_DEFINITION('material property','density of part',#10696);
#6219=PROPERTY_DEFINITION('material property','material name',#10697);
#6220=PROPERTY_DEFINITION('material property','density of part',#10697);
#6221=PROPERTY_DEFINITION('material property','material name',#10698);
#6222=PROPERTY_DEFINITION('material property','density of part',#10698);
#6223=PROPERTY_DEFINITION('material property','material name',#10700);
#6224=PROPERTY_DEFINITION('material property','density of part',#10700);
#6225=PROPERTY_DEFINITION('material property','material name',#10701);
#6226=PROPERTY_DEFINITION('material property','density of part',#10701);
#6227=PROPERTY_DEFINITION('material property','material name',#10702);
#6228=PROPERTY_DEFINITION('material property','density of part',#10702);
#6229=PROPERTY_DEFINITION('material property','material name',#10703);
#6230=PROPERTY_DEFINITION('material property','density of part',#10703);
#6231=PROPERTY_DEFINITION('material property','material name',#10704);
#6232=PROPERTY_DEFINITION('material property','density of part',#10704);
#6233=PROPERTY_DEFINITION('material property','material name',#10705);
#6234=PROPERTY_DEFINITION('material property','density of part',#10705);
#6235=AXIS2_PLACEMENT_3D('',#8766,#6924,#6925);
#6236=AXIS2_PLACEMENT_3D('',#8767,#6926,#6927);
#6237=AXIS2_PLACEMENT_3D('',#8768,#6928,#6929);
#6238=AXIS2_PLACEMENT_3D('',#8769,#6930,#6931);
#6239=AXIS2_PLACEMENT_3D('',#8771,#6932,#6933);
#6240=AXIS2_PLACEMENT_3D('',#8774,#6935,#6936);
#6241=AXIS2_PLACEMENT_3D('',#8775,#6937,#6938);
#6242=AXIS2_PLACEMENT_3D('',#8777,#6939,#6940);
#6243=AXIS2_PLACEMENT_3D('',#8778,#6941,#6942);
#6244=AXIS2_PLACEMENT_3D('',#8780,#6943,#6944);
#6245=AXIS2_PLACEMENT_3D('',#8783,#6946,#6947);
#6246=AXIS2_PLACEMENT_3D('',#8784,#6948,#6949);
#6247=AXIS2_PLACEMENT_3D('',#8786,#6950,#6951);
#6248=AXIS2_PLACEMENT_3D('',#8787,#6952,#6953);
#6249=AXIS2_PLACEMENT_3D('',#8789,#6955,#6956);
#6250=AXIS2_PLACEMENT_3D('',#8791,#6957,#6958);
#6251=AXIS2_PLACEMENT_3D('',#8794,#6960,#6961);
#6252=AXIS2_PLACEMENT_3D('',#8795,#6962,#6963);
#6253=AXIS2_PLACEMENT_3D('',#8796,#6964,#6965);
#6254=AXIS2_PLACEMENT_3D('',#8797,#6966,#6967);
#6255=AXIS2_PLACEMENT_3D('',#8798,#6968,#6969);
#6256=AXIS2_PLACEMENT_3D('',#8800,#6970,#6971);
#6257=AXIS2_PLACEMENT_3D('',#8803,#6973,#6974);
#6258=AXIS2_PLACEMENT_3D('',#8804,#6975,#6976);
#6259=AXIS2_PLACEMENT_3D('',#8806,#6977,#6978);
#6260=AXIS2_PLACEMENT_3D('',#8807,#6979,#6980);
#6261=AXIS2_PLACEMENT_3D('',#8809,#6981,#6982);
#6262=AXIS2_PLACEMENT_3D('',#8812,#6984,#6985);
#6263=AXIS2_PLACEMENT_3D('',#8813,#6986,#6987);
#6264=AXIS2_PLACEMENT_3D('',#8815,#6988,#6989);
#6265=AXIS2_PLACEMENT_3D('',#8816,#6990,#6991);
#6266=AXIS2_PLACEMENT_3D('',#8818,#6993,#6994);
#6267=AXIS2_PLACEMENT_3D('',#8820,#6995,#6996);
#6268=AXIS2_PLACEMENT_3D('',#8823,#6998,#6999);
#6269=AXIS2_PLACEMENT_3D('',#8824,#7000,#7001);
#6270=AXIS2_PLACEMENT_3D('',#8825,#7002,#7003);
#6271=AXIS2_PLACEMENT_3D('',#8826,#7004,#7005);
#6272=AXIS2_PLACEMENT_3D('',#8827,#7006,#7007);
#6273=AXIS2_PLACEMENT_3D('',#8829,#7008,#7009);
#6274=AXIS2_PLACEMENT_3D('',#8832,#7011,#7012);
#6275=AXIS2_PLACEMENT_3D('',#8833,#7013,#7014);
#6276=AXIS2_PLACEMENT_3D('',#8835,#7015,#7016);
#6277=AXIS2_PLACEMENT_3D('',#8838,#7018,#7019);
#6278=AXIS2_PLACEMENT_3D('',#8839,#7020,#7021);
#6279=AXIS2_PLACEMENT_3D('',#8841,#7022,#7023);
#6280=AXIS2_PLACEMENT_3D('',#8844,#7025,#7026);
#6281=AXIS2_PLACEMENT_3D('',#8845,#7027,#7028);
#6282=AXIS2_PLACEMENT_3D('',#8847,#7029,#7030);
#6283=AXIS2_PLACEMENT_3D('',#8850,#7032,#7033);
#6284=AXIS2_PLACEMENT_3D('',#8851,#7034,#7035);
#6285=AXIS2_PLACEMENT_3D('',#8853,#7036,#7037);
#6286=AXIS2_PLACEMENT_3D('',#8856,#7039,#7040);
#6287=AXIS2_PLACEMENT_3D('',#8857,#7041,#7042);
#6288=AXIS2_PLACEMENT_3D('',#8859,#7043,#7044);
#6289=AXIS2_PLACEMENT_3D('',#8862,#7046,#7047);
#6290=AXIS2_PLACEMENT_3D('',#8863,#7048,#7049);
#6291=AXIS2_PLACEMENT_3D('',#8864,#7050,#7051);
#6292=AXIS2_PLACEMENT_3D('',#8866,#7052,#7053);
#6293=AXIS2_PLACEMENT_3D('',#8869,#7055,#7056);
#6294=AXIS2_PLACEMENT_3D('',#8870,#7057,#7058);
#6295=AXIS2_PLACEMENT_3D('',#8871,#7059,#7060);
#6296=AXIS2_PLACEMENT_3D('',#8873,#7061,#7062);
#6297=AXIS2_PLACEMENT_3D('',#8876,#7064,#7065);
#6298=AXIS2_PLACEMENT_3D('',#8877,#7066,#7067);
#6299=AXIS2_PLACEMENT_3D('',#8886,#7072,#7073);
#6300=AXIS2_PLACEMENT_3D('',#8895,#7078,#7079);
#6301=AXIS2_PLACEMENT_3D('',#8905,#7085,#7086);
#6302=AXIS2_PLACEMENT_3D('',#8906,#7087,#7088);
#6303=AXIS2_PLACEMENT_3D('',#8907,#7089,#7090);
#6304=AXIS2_PLACEMENT_3D('',#8908,#7091,#7092);
#6305=AXIS2_PLACEMENT_3D('',#8912,#7095,#7096);
#6306=AXIS2_PLACEMENT_3D('',#8918,#7100,#7101);
#6307=AXIS2_PLACEMENT_3D('',#8920,#7103,#7104);
#6308=AXIS2_PLACEMENT_3D('',#8924,#7107,#7108);
#6309=AXIS2_PLACEMENT_3D('',#8926,#7110,#7111);
#6310=AXIS2_PLACEMENT_3D('',#8928,#7112,#7113);
#6311=AXIS2_PLACEMENT_3D('',#8931,#7115,#7116);
#6312=AXIS2_PLACEMENT_3D('',#8932,#7117,#7118);
#6313=AXIS2_PLACEMENT_3D('',#8933,#7119,#7120);
#6314=AXIS2_PLACEMENT_3D('',#8935,#7121,#7122);
#6315=AXIS2_PLACEMENT_3D('',#8938,#7124,#7125);
#6316=AXIS2_PLACEMENT_3D('',#8939,#7126,#7127);
#6317=AXIS2_PLACEMENT_3D('',#8948,#7132,#7133);
#6318=AXIS2_PLACEMENT_3D('',#8957,#7138,#7139);
#6319=AXIS2_PLACEMENT_3D('',#8967,#7145,#7146);
#6320=AXIS2_PLACEMENT_3D('',#8968,#7147,#7148);
#6321=AXIS2_PLACEMENT_3D('',#8969,#7149,#7150);
#6322=AXIS2_PLACEMENT_3D('',#8970,#7151,#7152);
#6323=AXIS2_PLACEMENT_3D('',#8974,#7155,#7156);
#6324=AXIS2_PLACEMENT_3D('',#8980,#7160,#7161);
#6325=AXIS2_PLACEMENT_3D('',#8982,#7163,#7164);
#6326=AXIS2_PLACEMENT_3D('',#8986,#7167,#7168);
#6327=AXIS2_PLACEMENT_3D('',#8988,#7170,#7171);
#6328=AXIS2_PLACEMENT_3D('',#8997,#7176,#7177);
#6329=AXIS2_PLACEMENT_3D('',#9003,#7181,#7182);
#6330=AXIS2_PLACEMENT_3D('',#9009,#7186,#7187);
#6331=AXIS2_PLACEMENT_3D('',#9012,#7190,#7191);
#6332=AXIS2_PLACEMENT_3D('',#9013,#7192,#7193);
#6333=AXIS2_PLACEMENT_3D('',#9014,#7194,#7195);
#6334=AXIS2_PLACEMENT_3D('',#9015,#7196,#7197);
#6335=AXIS2_PLACEMENT_3D('',#9017,#7198,#7199);
#6336=AXIS2_PLACEMENT_3D('',#9020,#7201,#7202);
#6337=AXIS2_PLACEMENT_3D('',#9021,#7203,#7204);
#6338=AXIS2_PLACEMENT_3D('',#9030,#7209,#7210);
#6339=AXIS2_PLACEMENT_3D('',#9036,#7214,#7215);
#6340=AXIS2_PLACEMENT_3D('',#9042,#7219,#7220);
#6341=AXIS2_PLACEMENT_3D('',#9048,#7224,#7225);
#6342=AXIS2_PLACEMENT_3D('',#9054,#7229,#7230);
#6343=AXIS2_PLACEMENT_3D('',#9057,#7233,#7234);
#6344=AXIS2_PLACEMENT_3D('',#9058,#7235,#7236);
#6345=AXIS2_PLACEMENT_3D('',#9059,#7237,#7238);
#6346=AXIS2_PLACEMENT_3D('',#9060,#7239,#7240);
#6347=AXIS2_PLACEMENT_3D('',#9062,#7241,#7242);
#6348=AXIS2_PLACEMENT_3D('',#9064,#7243,#7244);
#6349=AXIS2_PLACEMENT_3D('',#9065,#7245,#7246);
#6350=AXIS2_PLACEMENT_3D('',#9067,#7247,#7248);
#6351=AXIS2_PLACEMENT_3D('',#9069,#7250,#7251);
#6352=AXIS2_PLACEMENT_3D('',#9071,#7252,#7253);
#6353=AXIS2_PLACEMENT_3D('',#9072,#7254,#7255);
#6354=AXIS2_PLACEMENT_3D('',#9074,#7256,#7257);
#6355=AXIS2_PLACEMENT_3D('',#9076,#7259,#7260);
#6356=AXIS2_PLACEMENT_3D('',#9078,#7261,#7262);
#6357=AXIS2_PLACEMENT_3D('',#9080,#7264,#7265);
#6358=AXIS2_PLACEMENT_3D('',#9082,#7266,#7267);
#6359=AXIS2_PLACEMENT_3D('',#9083,#7268,#7269);
#6360=AXIS2_PLACEMENT_3D('',#9085,#7270,#7271);
#6361=AXIS2_PLACEMENT_3D('',#9087,#7273,#7274);
#6362=AXIS2_PLACEMENT_3D('',#9089,#7275,#7276);
#6363=AXIS2_PLACEMENT_3D('',#9091,#7278,#7279);
#6364=AXIS2_PLACEMENT_3D('',#9093,#7280,#7281);
#6365=AXIS2_PLACEMENT_3D('',#9094,#7282,#7283);
#6366=AXIS2_PLACEMENT_3D('',#9096,#7284,#7285);
#6367=AXIS2_PLACEMENT_3D('',#9098,#7287,#7288);
#6368=AXIS2_PLACEMENT_3D('',#9100,#7289,#7290);
#6369=AXIS2_PLACEMENT_3D('',#9102,#7292,#7293);
#6370=AXIS2_PLACEMENT_3D('',#9116,#7300,#7301);
#6371=AXIS2_PLACEMENT_3D('',#9117,#7302,#7303);
#6372=AXIS2_PLACEMENT_3D('',#9123,#7307,#7308);
#6373=AXIS2_PLACEMENT_3D('',#9127,#7311,#7312);
#6374=AXIS2_PLACEMENT_3D('',#9131,#7315,#7316);
#6375=AXIS2_PLACEMENT_3D('',#9135,#7319,#7320);
#6376=AXIS2_PLACEMENT_3D('',#9139,#7323,#7324);
#6377=AXIS2_PLACEMENT_3D('',#9141,#7326,#7327);
#6378=AXIS2_PLACEMENT_3D('',#9142,#7328,#7329);
#6379=AXIS2_PLACEMENT_3D('',#9145,#7331,#7332);
#6380=AXIS2_PLACEMENT_3D('',#9146,#7333,#7334);
#6381=AXIS2_PLACEMENT_3D('',#9147,#7335,#7336);
#6382=AXIS2_PLACEMENT_3D('',#9148,#7337,#7338);
#6383=AXIS2_PLACEMENT_3D('',#9150,#7339,#7340);
#6384=AXIS2_PLACEMENT_3D('',#9153,#7342,#7343);
#6385=AXIS2_PLACEMENT_3D('',#9154,#7344,#7345);
#6386=AXIS2_PLACEMENT_3D('',#9155,#7346,#7347);
#6387=AXIS2_PLACEMENT_3D('',#9157,#7348,#7349);
#6388=AXIS2_PLACEMENT_3D('',#9160,#7351,#7352);
#6389=AXIS2_PLACEMENT_3D('',#9161,#7353,#7354);
#6390=AXIS2_PLACEMENT_3D('',#9162,#7355,#7356);
#6391=AXIS2_PLACEMENT_3D('',#9164,#7357,#7358);
#6392=AXIS2_PLACEMENT_3D('',#9167,#7360,#7361);
#6393=AXIS2_PLACEMENT_3D('',#9168,#7362,#7363);
#6394=AXIS2_PLACEMENT_3D('',#9170,#7364,#7365);
#6395=AXIS2_PLACEMENT_3D('',#9173,#7367,#7368);
#6396=AXIS2_PLACEMENT_3D('',#9174,#7369,#7370);
#6397=AXIS2_PLACEMENT_3D('',#9176,#7371,#7372);
#6398=AXIS2_PLACEMENT_3D('',#9179,#7374,#7375);
#6399=AXIS2_PLACEMENT_3D('',#9180,#7376,#7377);
#6400=AXIS2_PLACEMENT_3D('',#9182,#7378,#7379);
#6401=AXIS2_PLACEMENT_3D('',#9185,#7381,#7382);
#6402=AXIS2_PLACEMENT_3D('',#9186,#7383,#7384);
#6403=AXIS2_PLACEMENT_3D('',#9191,#7386,#7387);
#6404=AXIS2_PLACEMENT_3D('',#9194,#7389,#7390);
#6405=AXIS2_PLACEMENT_3D('',#9195,#7391,#7392);
#6406=AXIS2_PLACEMENT_3D('',#9199,#7394,#7395);
#6407=AXIS2_PLACEMENT_3D('',#9201,#7397,#7398);
#6408=AXIS2_PLACEMENT_3D('',#9211,#7404,#7405);
#6409=AXIS2_PLACEMENT_3D('',#9213,#7406,#7407);
#6410=AXIS2_PLACEMENT_3D('',#9216,#7409,#7410);
#6411=AXIS2_PLACEMENT_3D('',#9217,#7411,#7412);
#6412=AXIS2_PLACEMENT_3D('',#9219,#7413,#7414);
#6413=AXIS2_PLACEMENT_3D('',#9222,#7416,#7417);
#6414=AXIS2_PLACEMENT_3D('',#9223,#7418,#7419);
#6415=AXIS2_PLACEMENT_3D('',#9225,#7420,#7421);
#6416=AXIS2_PLACEMENT_3D('',#9226,#7422,#7423);
#6417=AXIS2_PLACEMENT_3D('',#9227,#7424,#7425);
#6418=AXIS2_PLACEMENT_3D('',#9228,#7426,#7427);
#6419=AXIS2_PLACEMENT_3D('',#9229,#7428,#7429);
#6420=AXIS2_PLACEMENT_3D('',#9235,#7433,#7434);
#6421=AXIS2_PLACEMENT_3D('',#9239,#7437,#7438);
#6422=AXIS2_PLACEMENT_3D('',#9243,#7441,#7442);
#6423=AXIS2_PLACEMENT_3D('',#9245,#7444,#7445);
#6424=AXIS2_PLACEMENT_3D('',#9246,#7446,#7447);
#6425=AXIS2_PLACEMENT_3D('',#9247,#7448,#7449);
#6426=AXIS2_PLACEMENT_3D('',#9249,#7450,#7451);
#6427=AXIS2_PLACEMENT_3D('',#9252,#7453,#7454);
#6428=AXIS2_PLACEMENT_3D('',#9253,#7455,#7456);
#6429=AXIS2_PLACEMENT_3D('',#9254,#7457,#7458);
#6430=AXIS2_PLACEMENT_3D('',#9256,#7459,#7460);
#6431=AXIS2_PLACEMENT_3D('',#9259,#7462,#7463);
#6432=AXIS2_PLACEMENT_3D('',#9260,#7464,#7465);
#6433=AXIS2_PLACEMENT_3D('',#9261,#7466,#7467);
#6434=AXIS2_PLACEMENT_3D('',#9263,#7468,#7469);
#6435=AXIS2_PLACEMENT_3D('',#9266,#7471,#7472);
#6436=AXIS2_PLACEMENT_3D('',#9267,#7473,#7474);
#6437=AXIS2_PLACEMENT_3D('',#9269,#7475,#7476);
#6438=AXIS2_PLACEMENT_3D('',#9272,#7478,#7479);
#6439=AXIS2_PLACEMENT_3D('',#9273,#7480,#7481);
#6440=AXIS2_PLACEMENT_3D('',#9275,#7482,#7483);
#6441=AXIS2_PLACEMENT_3D('',#9278,#7485,#7486);
#6442=AXIS2_PLACEMENT_3D('',#9279,#7487,#7488);
#6443=AXIS2_PLACEMENT_3D('',#9281,#7489,#7490);
#6444=AXIS2_PLACEMENT_3D('',#9284,#7492,#7493);
#6445=AXIS2_PLACEMENT_3D('',#9285,#7494,#7495);
#6446=AXIS2_PLACEMENT_3D('',#9290,#7497,#7498);
#6447=AXIS2_PLACEMENT_3D('',#9293,#7500,#7501);
#6448=AXIS2_PLACEMENT_3D('',#9294,#7502,#7503);
#6449=AXIS2_PLACEMENT_3D('',#9298,#7505,#7506);
#6450=AXIS2_PLACEMENT_3D('',#9300,#7508,#7509);
#6451=AXIS2_PLACEMENT_3D('',#9310,#7515,#7516);
#6452=AXIS2_PLACEMENT_3D('',#9312,#7517,#7518);
#6453=AXIS2_PLACEMENT_3D('',#9315,#7520,#7521);
#6454=AXIS2_PLACEMENT_3D('',#9316,#7522,#7523);
#6455=AXIS2_PLACEMENT_3D('',#9318,#7524,#7525);
#6456=AXIS2_PLACEMENT_3D('',#9321,#7527,#7528);
#6457=AXIS2_PLACEMENT_3D('',#9322,#7529,#7530);
#6458=AXIS2_PLACEMENT_3D('',#9323,#7531,#7532);
#6459=AXIS2_PLACEMENT_3D('',#9325,#7533,#7534);
#6460=AXIS2_PLACEMENT_3D('',#9326,#7535,#7536);
#6461=AXIS2_PLACEMENT_3D('',#9327,#7537,#7538);
#6462=AXIS2_PLACEMENT_3D('',#9328,#7539,#7540);
#6463=AXIS2_PLACEMENT_3D('',#9334,#7544,#7545);
#6464=AXIS2_PLACEMENT_3D('',#9338,#7548,#7549);
#6465=AXIS2_PLACEMENT_3D('',#9342,#7552,#7553);
#6466=AXIS2_PLACEMENT_3D('',#9344,#7555,#7556);
#6467=AXIS2_PLACEMENT_3D('',#9345,#7557,#7558);
#6468=AXIS2_PLACEMENT_3D('',#9346,#7559,#7560);
#6469=AXIS2_PLACEMENT_3D('',#9348,#7561,#7562);
#6470=AXIS2_PLACEMENT_3D('',#9351,#7564,#7565);
#6471=AXIS2_PLACEMENT_3D('',#9352,#7566,#7567);
#6472=AXIS2_PLACEMENT_3D('',#9354,#7568,#7569);
#6473=AXIS2_PLACEMENT_3D('',#9357,#7571,#7572);
#6474=AXIS2_PLACEMENT_3D('',#9358,#7573,#7574);
#6475=AXIS2_PLACEMENT_3D('',#9360,#7575,#7576);
#6476=AXIS2_PLACEMENT_3D('',#9363,#7578,#7579);
#6477=AXIS2_PLACEMENT_3D('',#9364,#7580,#7581);
#6478=AXIS2_PLACEMENT_3D('',#9366,#7582,#7583);
#6479=AXIS2_PLACEMENT_3D('',#9369,#7585,#7586);
#6480=AXIS2_PLACEMENT_3D('',#9370,#7587,#7588);
#6481=AXIS2_PLACEMENT_3D('',#9379,#7593,#7594);
#6482=AXIS2_PLACEMENT_3D('',#9388,#7599,#7600);
#6483=AXIS2_PLACEMENT_3D('',#9394,#7604,#7605);
#6484=AXIS2_PLACEMENT_3D('',#9400,#7609,#7610);
#6485=AXIS2_PLACEMENT_3D('',#9401,#7611,#7612);
#6486=AXIS2_PLACEMENT_3D('',#9411,#7618,#7619);
#6487=AXIS2_PLACEMENT_3D('',#9415,#7622,#7623);
#6488=AXIS2_PLACEMENT_3D('',#9419,#7626,#7627);
#6489=AXIS2_PLACEMENT_3D('',#9420,#7628,#7629);
#6490=AXIS2_PLACEMENT_3D('',#9421,#7630,#7631);
#6491=AXIS2_PLACEMENT_3D('',#9425,#7634,#7635);
#6492=AXIS2_PLACEMENT_3D('',#9429,#7638,#7639);
#6493=AXIS2_PLACEMENT_3D('',#9431,#7641,#7642);
#6494=AXIS2_PLACEMENT_3D('',#9432,#7643,#7644);
#6495=AXIS2_PLACEMENT_3D('',#9433,#7645,#7646);
#6496=AXIS2_PLACEMENT_3D('',#9435,#7647,#7648);
#6497=AXIS2_PLACEMENT_3D('',#9437,#7649,#7650);
#6498=AXIS2_PLACEMENT_3D('',#9438,#7651,#7652);
#6499=AXIS2_PLACEMENT_3D('',#9440,#7653,#7654);
#6500=AXIS2_PLACEMENT_3D('',#9442,#7656,#7657);
#6501=AXIS2_PLACEMENT_3D('',#9444,#7658,#7659);
#6502=AXIS2_PLACEMENT_3D('',#9445,#7660,#7661);
#6503=AXIS2_PLACEMENT_3D('',#9448,#7663,#7664);
#6504=AXIS2_PLACEMENT_3D('',#9449,#7665,#7666);
#6505=AXIS2_PLACEMENT_3D('',#9452,#7668,#7669);
#6506=AXIS2_PLACEMENT_3D('',#9453,#7670,#7671);
#6507=AXIS2_PLACEMENT_3D('',#9454,#7672,#7673);
#6508=AXIS2_PLACEMENT_3D('',#9455,#7674,#7675);
#6509=AXIS2_PLACEMENT_3D('',#9457,#7676,#7677);
#6510=AXIS2_PLACEMENT_3D('',#9458,#7678,#7679);
#6511=AXIS2_PLACEMENT_3D('',#9459,#7680,#7681);
#6512=AXIS2_PLACEMENT_3D('',#9460,#7682,#7683);
#6513=AXIS2_PLACEMENT_3D('',#9462,#7684,#7685);
#6514=AXIS2_PLACEMENT_3D('',#9465,#7687,#7688);
#6515=AXIS2_PLACEMENT_3D('',#9466,#7689,#7690);
#6516=AXIS2_PLACEMENT_3D('',#9468,#7691,#7692);
#6517=AXIS2_PLACEMENT_3D('',#9469,#7693,#7694);
#6518=AXIS2_PLACEMENT_3D('',#9471,#7695,#7696);
#6519=AXIS2_PLACEMENT_3D('',#9473,#7698,#7699);
#6520=AXIS2_PLACEMENT_3D('',#9475,#7700,#7701);
#6521=AXIS2_PLACEMENT_3D('',#9478,#7703,#7704);
#6522=AXIS2_PLACEMENT_3D('',#9479,#7705,#7706);
#6523=AXIS2_PLACEMENT_3D('',#9480,#7707,#7708);
#6524=AXIS2_PLACEMENT_3D('',#9481,#7709,#7710);
#6525=AXIS2_PLACEMENT_3D('',#9482,#7711,#7712);
#6526=AXIS2_PLACEMENT_3D('',#9484,#7713,#7714);
#6527=AXIS2_PLACEMENT_3D('',#9487,#7716,#7717);
#6528=AXIS2_PLACEMENT_3D('',#9488,#7718,#7719);
#6529=AXIS2_PLACEMENT_3D('',#9489,#7720,#7721);
#6530=AXIS2_PLACEMENT_3D('',#9491,#7722,#7723);
#6531=AXIS2_PLACEMENT_3D('',#9494,#7725,#7726);
#6532=AXIS2_PLACEMENT_3D('',#9495,#7727,#7728);
#6533=AXIS2_PLACEMENT_3D('',#9496,#7729,#7730);
#6534=AXIS2_PLACEMENT_3D('',#9498,#7731,#7732);
#6535=AXIS2_PLACEMENT_3D('',#9501,#7734,#7735);
#6536=AXIS2_PLACEMENT_3D('',#9502,#7736,#7737);
#6537=AXIS2_PLACEMENT_3D('',#9504,#7738,#7739);
#6538=AXIS2_PLACEMENT_3D('',#9507,#7741,#7742);
#6539=AXIS2_PLACEMENT_3D('',#9508,#7743,#7744);
#6540=AXIS2_PLACEMENT_3D('',#9510,#7745,#7746);
#6541=AXIS2_PLACEMENT_3D('',#9513,#7748,#7749);
#6542=AXIS2_PLACEMENT_3D('',#9514,#7750,#7751);
#6543=AXIS2_PLACEMENT_3D('',#9516,#7752,#7753);
#6544=AXIS2_PLACEMENT_3D('',#9519,#7755,#7756);
#6545=AXIS2_PLACEMENT_3D('',#9520,#7757,#7758);
#6546=AXIS2_PLACEMENT_3D('',#9522,#7759,#7760);
#6547=AXIS2_PLACEMENT_3D('',#9525,#7762,#7763);
#6548=AXIS2_PLACEMENT_3D('',#9526,#7764,#7765);
#6549=AXIS2_PLACEMENT_3D('',#9535,#7770,#7771);
#6550=AXIS2_PLACEMENT_3D('',#9541,#7775,#7776);
#6551=AXIS2_PLACEMENT_3D('',#9547,#7780,#7781);
#6552=AXIS2_PLACEMENT_3D('',#9550,#7784,#7785);
#6553=AXIS2_PLACEMENT_3D('',#9551,#7786,#7787);
#6554=AXIS2_PLACEMENT_3D('',#9552,#7788,#7789);
#6555=AXIS2_PLACEMENT_3D('',#9553,#7790,#7791);
#6556=AXIS2_PLACEMENT_3D('',#9555,#7792,#7793);
#6557=AXIS2_PLACEMENT_3D('',#9557,#7794,#7795);
#6558=AXIS2_PLACEMENT_3D('',#9558,#7796,#7797);
#6559=AXIS2_PLACEMENT_3D('',#9561,#7799,#7800);
#6560=AXIS2_PLACEMENT_3D('',#9562,#7801,#7802);
#6561=AXIS2_PLACEMENT_3D('',#9564,#7803,#7804);
#6562=AXIS2_PLACEMENT_3D('',#9567,#7806,#7807);
#6563=AXIS2_PLACEMENT_3D('',#9568,#7808,#7809);
#6564=AXIS2_PLACEMENT_3D('',#9569,#7810,#7811);
#6565=AXIS2_PLACEMENT_3D('',#9570,#7812,#7813);
#6566=AXIS2_PLACEMENT_3D('',#9571,#7814,#7815);
#6567=AXIS2_PLACEMENT_3D('',#9580,#7820,#7821);
#6568=AXIS2_PLACEMENT_3D('',#9586,#7825,#7826);
#6569=AXIS2_PLACEMENT_3D('',#9592,#7830,#7831);
#6570=AXIS2_PLACEMENT_3D('',#9598,#7835,#7836);
#6571=AXIS2_PLACEMENT_3D('',#9604,#7840,#7841);
#6572=AXIS2_PLACEMENT_3D('',#9607,#7844,#7845);
#6573=AXIS2_PLACEMENT_3D('',#9608,#7846,#7847);
#6574=AXIS2_PLACEMENT_3D('',#9609,#7848,#7849);
#6575=AXIS2_PLACEMENT_3D('',#9611,#7850,#7851);
#6576=AXIS2_PLACEMENT_3D('',#9613,#7852,#7853);
#6577=AXIS2_PLACEMENT_3D('',#9614,#7854,#7855);
#6578=AXIS2_PLACEMENT_3D('',#9617,#7857,#7858);
#6579=AXIS2_PLACEMENT_3D('',#9618,#7859,#7860);
#6580=AXIS2_PLACEMENT_3D('',#9619,#7861,#7862);
#6581=AXIS2_PLACEMENT_3D('',#9621,#7863,#7864);
#6582=AXIS2_PLACEMENT_3D('',#9622,#7865,#7866);
#6583=AXIS2_PLACEMENT_3D('',#9624,#7867,#7868);
#6584=AXIS2_PLACEMENT_3D('',#9626,#7870,#7871);
#6585=AXIS2_PLACEMENT_3D('',#9628,#7872,#7873);
#6586=AXIS2_PLACEMENT_3D('',#9630,#7875,#7876);
#6587=AXIS2_PLACEMENT_3D('',#9632,#7877,#7878);
#6588=AXIS2_PLACEMENT_3D('',#9634,#7880,#7881);
#6589=AXIS2_PLACEMENT_3D('',#9636,#7882,#7883);
#6590=AXIS2_PLACEMENT_3D('',#9637,#7884,#7885);
#6591=AXIS2_PLACEMENT_3D('',#9639,#7886,#7887);
#6592=AXIS2_PLACEMENT_3D('',#9641,#7889,#7890);
#6593=AXIS2_PLACEMENT_3D('',#9643,#7892,#7893);
#6594=AXIS2_PLACEMENT_3D('',#9644,#7894,#7895);
#6595=AXIS2_PLACEMENT_3D('',#9646,#7896,#7897);
#6596=AXIS2_PLACEMENT_3D('',#9649,#7899,#7900);
#6597=AXIS2_PLACEMENT_3D('',#9650,#7901,#7902);
#6598=AXIS2_PLACEMENT_3D('',#9653,#7904,#7905);
#6599=AXIS2_PLACEMENT_3D('',#9654,#7906,#7907);
#6600=AXIS2_PLACEMENT_3D('',#9656,#7908,#7909);
#6601=AXIS2_PLACEMENT_3D('',#9657,#7910,#7911);
#6602=AXIS2_PLACEMENT_3D('',#9660,#7913,#7914);
#6603=AXIS2_PLACEMENT_3D('',#9661,#7915,#7916);
#6604=AXIS2_PLACEMENT_3D('',#9662,#7917,#7918);
#6605=AXIS2_PLACEMENT_3D('',#9663,#7919,#7920);
#6606=AXIS2_PLACEMENT_3D('',#9675,#7922,#7923);
#6607=AXIS2_PLACEMENT_3D('',#9691,#7924,#7925);
#6608=AXIS2_PLACEMENT_3D('',#9693,#7926,#7927);
#6609=AXIS2_PLACEMENT_3D('',#9719,#7929,#7930);
#6610=AXIS2_PLACEMENT_3D('',#9722,#7933,#7934);
#6611=AXIS2_PLACEMENT_3D('',#9724,#7936,#7937);
#6612=AXIS2_PLACEMENT_3D('',#9726,#7939,#7940);
#6613=AXIS2_PLACEMENT_3D('',#9728,#7941,#7942);
#6614=AXIS2_PLACEMENT_3D('',#9731,#7944,#7945);
#6615=AXIS2_PLACEMENT_3D('',#9732,#7946,#7947);
#6616=AXIS2_PLACEMENT_3D('',#9734,#7949,#7950);
#6617=AXIS2_PLACEMENT_3D('',#9736,#7952,#7953);
#6618=AXIS2_PLACEMENT_3D('',#9737,#7954,#7955);
#6619=AXIS2_PLACEMENT_3D('',#9738,#7956,#7957);
#6620=AXIS2_PLACEMENT_3D('',#9739,#7958,#7959);
#6621=AXIS2_PLACEMENT_3D('',#9740,#7960,#7961);
#6622=AXIS2_PLACEMENT_3D('',#9754,#7968,#7969);
#6623=AXIS2_PLACEMENT_3D('',#9755,#7970,#7971);
#6624=AXIS2_PLACEMENT_3D('',#9769,#7978,#7979);
#6625=AXIS2_PLACEMENT_3D('',#9770,#7980,#7981);
#6626=AXIS2_PLACEMENT_3D('',#9773,#7984,#7985);
#6627=AXIS2_PLACEMENT_3D('',#9775,#7987,#7988);
#6628=AXIS2_PLACEMENT_3D('',#9777,#7990,#7991);
#6629=AXIS2_PLACEMENT_3D('',#9779,#7993,#7994);
#6630=AXIS2_PLACEMENT_3D('',#9781,#7996,#7997);
#6631=AXIS2_PLACEMENT_3D('',#9782,#7998,#7999);
#6632=AXIS2_PLACEMENT_3D('',#9785,#8001,#8002);
#6633=AXIS2_PLACEMENT_3D('',#9786,#8003,#8004);
#6634=AXIS2_PLACEMENT_3D('',#9788,#8005,#8006);
#6635=AXIS2_PLACEMENT_3D('',#9790,#8007,#8008);
#6636=AXIS2_PLACEMENT_3D('',#9791,#8009,#8010);
#6637=AXIS2_PLACEMENT_3D('',#9793,#8012,#8013);
#6638=AXIS2_PLACEMENT_3D('',#9795,#8014,#8015);
#6639=AXIS2_PLACEMENT_3D('',#9797,#8017,#8018);
#6640=AXIS2_PLACEMENT_3D('',#9799,#8019,#8020);
#6641=AXIS2_PLACEMENT_3D('',#9801,#8022,#8023);
#6642=AXIS2_PLACEMENT_3D('',#9803,#8024,#8025);
#6643=AXIS2_PLACEMENT_3D('',#9804,#8026,#8027);
#6644=AXIS2_PLACEMENT_3D('',#9806,#8029,#8030);
#6645=AXIS2_PLACEMENT_3D('',#9807,#8031,#8032);
#6646=AXIS2_PLACEMENT_3D('',#9809,#8033,#8034);
#6647=AXIS2_PLACEMENT_3D('',#9812,#8036,#8037);
#6648=AXIS2_PLACEMENT_3D('',#9813,#8038,#8039);
#6649=AXIS2_PLACEMENT_3D('',#9815,#8040,#8041);
#6650=AXIS2_PLACEMENT_3D('',#9818,#8043,#8044);
#6651=AXIS2_PLACEMENT_3D('',#9819,#8045,#8046);
#6652=AXIS2_PLACEMENT_3D('',#9820,#8047,#8048);
#6653=AXIS2_PLACEMENT_3D('',#9821,#8049,#8050);
#6654=AXIS2_PLACEMENT_3D('',#9822,#8051,#8052);
#6655=AXIS2_PLACEMENT_3D('',#9824,#8053,#8054);
#6656=AXIS2_PLACEMENT_3D('',#9825,#8055,#8056);
#6657=AXIS2_PLACEMENT_3D('',#9827,#8057,#8058);
#6658=AXIS2_PLACEMENT_3D('',#9829,#8060,#8061);
#6659=AXIS2_PLACEMENT_3D('',#9831,#8062,#8063);
#6660=AXIS2_PLACEMENT_3D('',#9833,#8065,#8066);
#6661=AXIS2_PLACEMENT_3D('',#9835,#8067,#8068);
#6662=AXIS2_PLACEMENT_3D('',#9837,#8070,#8071);
#6663=AXIS2_PLACEMENT_3D('',#9839,#8072,#8073);
#6664=AXIS2_PLACEMENT_3D('',#9840,#8074,#8075);
#6665=AXIS2_PLACEMENT_3D('',#9842,#8076,#8077);
#6666=AXIS2_PLACEMENT_3D('',#9844,#8079,#8080);
#6667=AXIS2_PLACEMENT_3D('',#9846,#8081,#8082);
#6668=AXIS2_PLACEMENT_3D('',#9848,#8084,#8085);
#6669=AXIS2_PLACEMENT_3D('',#9850,#8086,#8087);
#6670=AXIS2_PLACEMENT_3D('',#9852,#8089,#8090);
#6671=AXIS2_PLACEMENT_3D('',#9853,#8091,#8092);
#6672=AXIS2_PLACEMENT_3D('',#9862,#8097,#8098);
#6673=AXIS2_PLACEMENT_3D('',#9868,#8102,#8103);
#6674=AXIS2_PLACEMENT_3D('',#9874,#8107,#8108);
#6675=AXIS2_PLACEMENT_3D('',#9880,#8112,#8113);
#6676=AXIS2_PLACEMENT_3D('',#9886,#8117,#8118);
#6677=AXIS2_PLACEMENT_3D('',#9889,#8121,#8122);
#6678=AXIS2_PLACEMENT_3D('',#9890,#8123,#8124);
#6679=AXIS2_PLACEMENT_3D('',#9891,#8125,#8126);
#6680=AXIS2_PLACEMENT_3D('',#9892,#8127,#8128);
#6681=AXIS2_PLACEMENT_3D('',#9894,#8129,#8130);
#6682=AXIS2_PLACEMENT_3D('',#9897,#8132,#8133);
#6683=AXIS2_PLACEMENT_3D('',#9898,#8134,#8135);
#6684=AXIS2_PLACEMENT_3D('',#9899,#8136,#8137);
#6685=AXIS2_PLACEMENT_3D('',#9900,#8138,#8139);
#6686=AXIS2_PLACEMENT_3D('',#9901,#8140,#8141);
#6687=AXIS2_PLACEMENT_3D('',#9904,#8142,#8143);
#6688=AXIS2_PLACEMENT_3D('',#9906,#8144,#8145);
#6689=AXIS2_PLACEMENT_3D('',#9909,#8147,#8148);
#6690=AXIS2_PLACEMENT_3D('',#9910,#8149,#8150);
#6691=AXIS2_PLACEMENT_3D('',#9911,#8151,#8152);
#6692=AXIS2_PLACEMENT_3D('',#9914,#8153,#8154);
#6693=AXIS2_PLACEMENT_3D('',#9916,#8155,#8156);
#6694=AXIS2_PLACEMENT_3D('',#9917,#8157,#8158);
#6695=AXIS2_PLACEMENT_3D('',#9918,#8159,#8160);
#6696=AXIS2_PLACEMENT_3D('',#9921,#8162,#8163);
#6697=AXIS2_PLACEMENT_3D('',#9922,#8164,#8165);
#6698=AXIS2_PLACEMENT_3D('',#9924,#8166,#8167);
#6699=AXIS2_PLACEMENT_3D('',#9925,#8168,#8169);
#6700=AXIS2_PLACEMENT_3D('',#9927,#8170,#8171);
#6701=AXIS2_PLACEMENT_3D('',#9929,#8173,#8174);
#6702=AXIS2_PLACEMENT_3D('',#9931,#8175,#8176);
#6703=AXIS2_PLACEMENT_3D('',#9934,#8178,#8179);
#6704=AXIS2_PLACEMENT_3D('',#9935,#8180,#8181);
#6705=AXIS2_PLACEMENT_3D('',#9936,#8182,#8183);
#6706=AXIS2_PLACEMENT_3D('',#9939,#8184,#8185);
#6707=AXIS2_PLACEMENT_3D('',#9941,#8186,#8187);
#6708=AXIS2_PLACEMENT_3D('',#9943,#8188,#8189);
#6709=AXIS2_PLACEMENT_3D('',#9944,#8190,#8191);
#6710=AXIS2_PLACEMENT_3D('',#9945,#8192,#8193);
#6711=AXIS2_PLACEMENT_3D('',#9946,#8194,#8195);
#6712=AXIS2_PLACEMENT_3D('',#9949,#8197,#8198);
#6713=AXIS2_PLACEMENT_3D('',#9950,#8199,#8200);
#6714=AXIS2_PLACEMENT_3D('',#9952,#8201,#8202);
#6715=AXIS2_PLACEMENT_3D('',#9953,#8203,#8204);
#6716=AXIS2_PLACEMENT_3D('',#9955,#8205,#8206);
#6717=AXIS2_PLACEMENT_3D('',#9957,#8208,#8209);
#6718=AXIS2_PLACEMENT_3D('',#9958,#8210,#8211);
#6719=AXIS2_PLACEMENT_3D('',#9960,#8212,#8213);
#6720=AXIS2_PLACEMENT_3D('',#9962,#8214,#8215);
#6721=AXIS2_PLACEMENT_3D('',#9963,#8216,#8217);
#6722=AXIS2_PLACEMENT_3D('',#9965,#8218,#8219);
#6723=AXIS2_PLACEMENT_3D('',#9967,#8221,#8222);
#6724=AXIS2_PLACEMENT_3D('',#9968,#8223,#8224);
#6725=AXIS2_PLACEMENT_3D('',#9970,#8226,#8227);
#6726=AXIS2_PLACEMENT_3D('',#9971,#8228,#8229);
#6727=AXIS2_PLACEMENT_3D('',#9985,#8236,#8237);
#6728=AXIS2_PLACEMENT_3D('',#9986,#8238,#8239);
#6729=AXIS2_PLACEMENT_3D('',#10000,#8246,#8247);
#6730=AXIS2_PLACEMENT_3D('',#10001,#8248,#8249);
#6731=AXIS2_PLACEMENT_3D('',#10004,#8252,#8253);
#6732=AXIS2_PLACEMENT_3D('',#10006,#8255,#8256);
#6733=AXIS2_PLACEMENT_3D('',#10008,#8258,#8259);
#6734=AXIS2_PLACEMENT_3D('',#10010,#8261,#8262);
#6735=AXIS2_PLACEMENT_3D('',#10012,#8264,#8265);
#6736=AXIS2_PLACEMENT_3D('',#10013,#8266,#8267);
#6737=AXIS2_PLACEMENT_3D('',#10016,#8269,#8270);
#6738=AXIS2_PLACEMENT_3D('',#10017,#8271,#8272);
#6739=AXIS2_PLACEMENT_3D('',#10019,#8273,#8274);
#6740=AXIS2_PLACEMENT_3D('',#10021,#8275,#8276);
#6741=AXIS2_PLACEMENT_3D('',#10022,#8277,#8278);
#6742=AXIS2_PLACEMENT_3D('',#10024,#8280,#8281);
#6743=AXIS2_PLACEMENT_3D('',#10026,#8282,#8283);
#6744=AXIS2_PLACEMENT_3D('',#10028,#8285,#8286);
#6745=AXIS2_PLACEMENT_3D('',#10030,#8287,#8288);
#6746=AXIS2_PLACEMENT_3D('',#10032,#8290,#8291);
#6747=AXIS2_PLACEMENT_3D('',#10034,#8292,#8293);
#6748=AXIS2_PLACEMENT_3D('',#10035,#8294,#8295);
#6749=AXIS2_PLACEMENT_3D('',#10037,#8297,#8298);
#6750=AXIS2_PLACEMENT_3D('',#10038,#8299,#8300);
#6751=AXIS2_PLACEMENT_3D('',#10040,#8301,#8302);
#6752=AXIS2_PLACEMENT_3D('',#10043,#8304,#8305);
#6753=AXIS2_PLACEMENT_3D('',#10044,#8306,#8307);
#6754=AXIS2_PLACEMENT_3D('',#10046,#8308,#8309);
#6755=AXIS2_PLACEMENT_3D('',#10048,#8311,#8312);
#6756=AXIS2_PLACEMENT_3D('',#10049,#8313,#8314);
#6757=AXIS2_PLACEMENT_3D('',#10051,#8315,#8316);
#6758=AXIS2_PLACEMENT_3D('',#10077,#8318,#8319);
#6759=AXIS2_PLACEMENT_3D('',#10083,#8323,#8324);
#6760=AXIS2_PLACEMENT_3D('',#10087,#8327,#8328);
#6761=AXIS2_PLACEMENT_3D('',#10091,#8331,#8332);
#6762=AXIS2_PLACEMENT_3D('',#10095,#8335,#8336);
#6763=AXIS2_PLACEMENT_3D('',#10099,#8339,#8340);
#6764=AXIS2_PLACEMENT_3D('',#10101,#8342,#8343);
#6765=AXIS2_PLACEMENT_3D('',#10102,#8344,#8345);
#6766=AXIS2_PLACEMENT_3D('',#10103,#8346,#8347);
#6767=AXIS2_PLACEMENT_3D('',#10104,#8348,#8349);
#6768=AXIS2_PLACEMENT_3D('',#10105,#8350,#8351);
#6769=AXIS2_PLACEMENT_3D('',#10106,#8352,#8353);
#6770=AXIS2_PLACEMENT_3D('',#10107,#8354,#8355);
#6771=AXIS2_PLACEMENT_3D('',#10108,#8356,#8357);
#6772=AXIS2_PLACEMENT_3D('',#10109,#8358,#8359);
#6773=AXIS2_PLACEMENT_3D('',#10110,#8360,#8361);
#6774=AXIS2_PLACEMENT_3D('',#10111,#8362,#8363);
#6775=AXIS2_PLACEMENT_3D('',#10112,#8364,#8365);
#6776=AXIS2_PLACEMENT_3D('',#10113,#8366,#8367);
#6777=AXIS2_PLACEMENT_3D('',#10114,#8368,#8369);
#6778=AXIS2_PLACEMENT_3D('',#10115,#8370,#8371);
#6779=AXIS2_PLACEMENT_3D('',#10116,#8372,#8373);
#6780=AXIS2_PLACEMENT_3D('',#10117,#8374,#8375);
#6781=AXIS2_PLACEMENT_3D('',#10118,#8376,#8377);
#6782=AXIS2_PLACEMENT_3D('',#10119,#8378,#8379);
#6783=AXIS2_PLACEMENT_3D('',#10120,#8380,#8381);
#6784=AXIS2_PLACEMENT_3D('',#10121,#8382,#8383);
#6785=AXIS2_PLACEMENT_3D('',#10122,#8384,#8385);
#6786=AXIS2_PLACEMENT_3D('',#10123,#8386,#8387);
#6787=AXIS2_PLACEMENT_3D('',#10124,#8388,#8389);
#6788=AXIS2_PLACEMENT_3D('',#10125,#8390,#8391);
#6789=AXIS2_PLACEMENT_3D('',#10126,#8392,#8393);
#6790=AXIS2_PLACEMENT_3D('',#10127,#8394,#8395);
#6791=AXIS2_PLACEMENT_3D('',#10128,#8396,#8397);
#6792=AXIS2_PLACEMENT_3D('',#10129,#8398,#8399);
#6793=AXIS2_PLACEMENT_3D('',#10130,#8400,#8401);
#6794=AXIS2_PLACEMENT_3D('',#10131,#8402,#8403);
#6795=AXIS2_PLACEMENT_3D('',#10132,#8404,#8405);
#6796=AXIS2_PLACEMENT_3D('',#10133,#8406,#8407);
#6797=AXIS2_PLACEMENT_3D('',#10134,#8408,#8409);
#6798=AXIS2_PLACEMENT_3D('',#10135,#8410,#8411);
#6799=AXIS2_PLACEMENT_3D('',#10136,#8412,#8413);
#6800=AXIS2_PLACEMENT_3D('',#10137,#8414,#8415);
#6801=AXIS2_PLACEMENT_3D('',#10138,#8416,#8417);
#6802=AXIS2_PLACEMENT_3D('',#10139,#8418,#8419);
#6803=AXIS2_PLACEMENT_3D('',#10140,#8420,#8421);
#6804=AXIS2_PLACEMENT_3D('',#10141,#8422,#8423);
#6805=AXIS2_PLACEMENT_3D('',#10142,#8424,#8425);
#6806=AXIS2_PLACEMENT_3D('',#10143,#8426,#8427);
#6807=AXIS2_PLACEMENT_3D('',#10144,#8428,#8429);
#6808=AXIS2_PLACEMENT_3D('',#10145,#8430,#8431);
#6809=AXIS2_PLACEMENT_3D('',#10146,#8432,#8433);
#6810=AXIS2_PLACEMENT_3D('',#10147,#8434,#8435);
#6811=AXIS2_PLACEMENT_3D('',#10148,#8436,#8437);
#6812=AXIS2_PLACEMENT_3D('',#10149,#8438,#8439);
#6813=AXIS2_PLACEMENT_3D('',#10150,#8440,#8441);
#6814=AXIS2_PLACEMENT_3D('',#10151,#8442,#8443);
#6815=AXIS2_PLACEMENT_3D('',#10152,#8444,#8445);
#6816=AXIS2_PLACEMENT_3D('',#10155,#8446,#8447);
#6817=AXIS2_PLACEMENT_3D('',#10161,#8451,#8452);
#6818=AXIS2_PLACEMENT_3D('',#10163,#8453,#8454);
#6819=AXIS2_PLACEMENT_3D('',#10168,#8457,#8458);
#6820=AXIS2_PLACEMENT_3D('',#10169,#8459,#8460);
#6821=AXIS2_PLACEMENT_3D('',#10171,#8461,#8462);
#6822=AXIS2_PLACEMENT_3D('',#10175,#8465,#8466);
#6823=AXIS2_PLACEMENT_3D('',#10176,#8467,#8468);
#6824=AXIS2_PLACEMENT_3D('',#10178,#8470,#8471);
#6825=AXIS2_PLACEMENT_3D('',#10179,#8472,#8473);
#6826=AXIS2_PLACEMENT_3D('',#10181,#8474,#8475);
#6827=AXIS2_PLACEMENT_3D('',#10184,#8477,#8478);
#6828=AXIS2_PLACEMENT_3D('',#10185,#8479,#8480);
#6829=AXIS2_PLACEMENT_3D('',#10187,#8481,#8482);
#6830=AXIS2_PLACEMENT_3D('',#10188,#8483,#8484);
#6831=AXIS2_PLACEMENT_3D('',#10189,#8485,#8486);
#6832=AXIS2_PLACEMENT_3D('',#10191,#8487,#8488);
#6833=AXIS2_PLACEMENT_3D('',#10194,#8490,#8491);
#6834=AXIS2_PLACEMENT_3D('',#10195,#8492,#8493);
#6835=AXIS2_PLACEMENT_3D('',#10196,#8494,#8495);
#6836=AXIS2_PLACEMENT_3D('',#10199,#8496,#8497);
#6837=AXIS2_PLACEMENT_3D('',#10203,#8500,#8501);
#6838=AXIS2_PLACEMENT_3D('',#10206,#8502,#8503);
#6839=AXIS2_PLACEMENT_3D('',#10210,#8506,#8507);
#6840=AXIS2_PLACEMENT_3D('',#10213,#8508,#8509);
#6841=AXIS2_PLACEMENT_3D('',#10217,#8512,#8513);
#6842=AXIS2_PLACEMENT_3D('',#10220,#8514,#8515);
#6843=AXIS2_PLACEMENT_3D('',#10224,#8518,#8519);
#6844=AXIS2_PLACEMENT_3D('',#10231,#8524,#8525);
#6845=AXIS2_PLACEMENT_3D('',#10236,#8529,#8530);
#6846=AXIS2_PLACEMENT_3D('',#10241,#8534,#8535);
#6847=AXIS2_PLACEMENT_3D('',#10244,#8538,#8539);
#6848=AXIS2_PLACEMENT_3D('',#10245,#8540,#8541);
#6849=AXIS2_PLACEMENT_3D('',#10246,#8542,#8543);
#6850=AXIS2_PLACEMENT_3D('',#10247,#8544,#8545);
#6851=AXIS2_PLACEMENT_3D('',#10249,#8546,#8547);
#6852=AXIS2_PLACEMENT_3D('',#10250,#8548,#8549);
#6853=AXIS2_PLACEMENT_3D('',#10251,#8550,#8551);
#6854=AXIS2_PLACEMENT_3D('',#10252,#8552,#8553);
#6855=AXIS2_PLACEMENT_3D('',#10253,#8554,#8555);
#6856=AXIS2_PLACEMENT_3D('',#10254,#8556,#8557);
#6857=AXIS2_PLACEMENT_3D('',#10255,#8558,#8559);
#6858=AXIS2_PLACEMENT_3D('',#10264,#8564,#8565);
#6859=AXIS2_PLACEMENT_3D('',#10270,#8569,#8570);
#6860=AXIS2_PLACEMENT_3D('',#10276,#8574,#8575);
#6861=AXIS2_PLACEMENT_3D('',#10279,#8578,#8579);
#6862=AXIS2_PLACEMENT_3D('',#10280,#8580,#8581);
#6863=AXIS2_PLACEMENT_3D('',#10283,#8583,#8584);
#6864=AXIS2_PLACEMENT_3D('',#10284,#8585,#8586);
#6865=AXIS2_PLACEMENT_3D('',#10285,#8587,#8588);
#6866=AXIS2_PLACEMENT_3D('',#10286,#8589,#8590);
#6867=AXIS2_PLACEMENT_3D('',#10295,#8595,#8596);
#6868=AXIS2_PLACEMENT_3D('',#10301,#8600,#8601);
#6869=AXIS2_PLACEMENT_3D('',#10307,#8605,#8606);
#6870=AXIS2_PLACEMENT_3D('',#10310,#8609,#8610);
#6871=AXIS2_PLACEMENT_3D('',#10319,#8615,#8616);
#6872=AXIS2_PLACEMENT_3D('',#10325,#8620,#8621);
#6873=AXIS2_PLACEMENT_3D('',#10331,#8625,#8626);
#6874=AXIS2_PLACEMENT_3D('',#10334,#8629,#8630);
#6875=AXIS2_PLACEMENT_3D('',#10335,#8631,#8632);
#6876=AXIS2_PLACEMENT_3D('',#10336,#8633,#8634);
#6877=AXIS2_PLACEMENT_3D('',#10337,#8635,#8636);
#6878=AXIS2_PLACEMENT_3D('',#10339,#8637,#8638);
#6879=AXIS2_PLACEMENT_3D('',#10342,#8640,#8641);
#6880=AXIS2_PLACEMENT_3D('',#10343,#8642,#8643);
#6881=AXIS2_PLACEMENT_3D('',#10345,#8644,#8645);
#6882=AXIS2_PLACEMENT_3D('',#10348,#8647,#8648);
#6883=AXIS2_PLACEMENT_3D('',#10349,#8649,#8650);
#6884=AXIS2_PLACEMENT_3D('',#10350,#8651,#8652);
#6885=AXIS2_PLACEMENT_3D('',#10351,#8653,#8654);
#6886=AXIS2_PLACEMENT_3D('',#10352,#8655,#8656);
#6887=AXIS2_PLACEMENT_3D('',#10361,#8661,#8662);
#6888=AXIS2_PLACEMENT_3D('',#10367,#8666,#8667);
#6889=AXIS2_PLACEMENT_3D('',#10373,#8671,#8672);
#6890=AXIS2_PLACEMENT_3D('',#10376,#8675,#8676);
#6891=AXIS2_PLACEMENT_3D('',#10377,#8677,#8678);
#6892=AXIS2_PLACEMENT_3D('',#10378,#8679,#8680);
#6893=AXIS2_PLACEMENT_3D('',#10379,#8681,#8682);
#6894=AXIS2_PLACEMENT_3D('',#10388,#8687,#8688);
#6895=AXIS2_PLACEMENT_3D('',#10394,#8692,#8693);
#6896=AXIS2_PLACEMENT_3D('',#10400,#8697,#8698);
#6897=AXIS2_PLACEMENT_3D('',#10406,#8702,#8703);
#6898=AXIS2_PLACEMENT_3D('',#10412,#8707,#8708);
#6899=AXIS2_PLACEMENT_3D('',#10415,#8711,#8712);
#6900=AXIS2_PLACEMENT_3D('',#10416,#8713,#8714);
#6901=AXIS2_PLACEMENT_3D('',#10417,#8715,#8716);
#6902=AXIS2_PLACEMENT_3D('',#10419,#8717,#8718);
#6903=AXIS2_PLACEMENT_3D('',#10420,#8719,#8720);
#6904=AXIS2_PLACEMENT_3D('',#10422,#8721,#8722);
#6905=AXIS2_PLACEMENT_3D('',#10423,#8723,#8724);
#6906=AXIS2_PLACEMENT_3D('',#10425,#8725,#8726);
#6907=AXIS2_PLACEMENT_3D('',#10427,#8728,#8729);
#6908=AXIS2_PLACEMENT_3D('',#10429,#8730,#8731);
#6909=AXIS2_PLACEMENT_3D('',#10431,#8733,#8734);
#6910=AXIS2_PLACEMENT_3D('',#10433,#8735,#8736);
#6911=AXIS2_PLACEMENT_3D('',#10435,#8738,#8739);
#6912=AXIS2_PLACEMENT_3D('',#10437,#8740,#8741);
#6913=AXIS2_PLACEMENT_3D('',#10438,#8742,#8743);
#6914=AXIS2_PLACEMENT_3D('',#10440,#8744,#8745);
#6915=AXIS2_PLACEMENT_3D('',#10442,#8747,#8748);
#6916=AXIS2_PLACEMENT_3D('',#10444,#8750,#8751);
#6917=AXIS2_PLACEMENT_3D('',#10445,#8752,#8753);
#6918=AXIS2_PLACEMENT_3D('',#10446,#8754,#8755);
#6919=AXIS2_PLACEMENT_3D('',#10447,#8756,#8757);
#6920=AXIS2_PLACEMENT_3D('',#10448,#8758,#8759);
#6921=AXIS2_PLACEMENT_3D('',#10449,#8760,#8761);
#6922=AXIS2_PLACEMENT_3D('',#10450,#8762,#8763);
#6923=AXIS2_PLACEMENT_3D('',#10451,#8764,#8765);
#6924=DIRECTION('axis',(0.,0.,1.));
#6925=DIRECTION('refdir',(1.,0.,0.));
#6926=DIRECTION('axis',(0.,0.,1.));
#6927=DIRECTION('refdir',(1.,0.,0.));
#6928=DIRECTION('axis',(0.,0.,1.));
#6929=DIRECTION('refdir',(1.,0.,0.));
#6930=DIRECTION('center_axis',(0.,1.,0.));
#6931=DIRECTION('ref_axis',(1.,0.,0.));
#6932=DIRECTION('center_axis',(0.,1.,0.));
#6933=DIRECTION('ref_axis',(1.,0.,0.));
#6934=DIRECTION('',(0.,1.,0.));
#6935=DIRECTION('center_axis',(0.,1.,0.));
#6936=DIRECTION('ref_axis',(1.,0.,0.));
#6937=DIRECTION('center_axis',(0.,1.,0.));
#6938=DIRECTION('ref_axis',(1.,0.,0.));
#6939=DIRECTION('center_axis',(0.,-1.,0.));
#6940=DIRECTION('ref_axis',(1.,0.,0.));
#6941=DIRECTION('center_axis',(0.,1.,0.));
#6942=DIRECTION('ref_axis',(1.,0.,0.));
#6943=DIRECTION('center_axis',(0.,1.,0.));
#6944=DIRECTION('ref_axis',(1.,0.,0.));
#6945=DIRECTION('',(0.,1.,0.));
#6946=DIRECTION('center_axis',(0.,-1.,0.));
#6947=DIRECTION('ref_axis',(1.,0.,0.));
#6948=DIRECTION('center_axis',(0.,1.,0.));
#6949=DIRECTION('ref_axis',(1.,0.,0.));
#6950=DIRECTION('center_axis',(0.,1.,0.));
#6951=DIRECTION('ref_axis',(1.,0.,0.));
#6952=DIRECTION('center_axis',(0.,1.,0.));
#6953=DIRECTION('ref_axis',(1.,0.,0.));
#6954=DIRECTION('',(0.,-1.,0.));
#6955=DIRECTION('center_axis',(0.,1.,0.));
#6956=DIRECTION('ref_axis',(1.,0.,0.));
#6957=DIRECTION('center_axis',(0.,1.,0.));
#6958=DIRECTION('ref_axis',(1.,0.,0.));
#6959=DIRECTION('',(0.,-1.,0.));
#6960=DIRECTION('center_axis',(0.,1.,0.));
#6961=DIRECTION('ref_axis',(1.,0.,0.));
#6962=DIRECTION('center_axis',(0.,1.,0.));
#6963=DIRECTION('ref_axis',(1.,0.,0.));
#6964=DIRECTION('center_axis',(0.,1.,0.));
#6965=DIRECTION('ref_axis',(1.,0.,0.));
#6966=DIRECTION('axis',(0.,0.,1.));
#6967=DIRECTION('refdir',(1.,0.,0.));
#6968=DIRECTION('center_axis',(0.,1.,0.));
#6969=DIRECTION('ref_axis',(1.,0.,0.));
#6970=DIRECTION('center_axis',(0.,1.,0.));
#6971=DIRECTION('ref_axis',(1.,0.,0.));
#6972=DIRECTION('',(0.,1.,0.));
#6973=DIRECTION('center_axis',(0.,-1.,0.));
#6974=DIRECTION('ref_axis',(1.,0.,0.));
#6975=DIRECTION('center_axis',(0.,1.,0.));
#6976=DIRECTION('ref_axis',(1.,0.,0.));
#6977=DIRECTION('center_axis',(0.,1.,0.));
#6978=DIRECTION('ref_axis',(1.,0.,0.));
#6979=DIRECTION('center_axis',(0.,1.,0.));
#6980=DIRECTION('ref_axis',(1.,0.,0.));
#6981=DIRECTION('center_axis',(0.,1.,0.));
#6982=DIRECTION('ref_axis',(1.,0.,0.));
#6983=DIRECTION('',(0.,1.,0.));
#6984=DIRECTION('center_axis',(0.,1.,0.));
#6985=DIRECTION('ref_axis',(1.,0.,0.));
#6986=DIRECTION('center_axis',(0.,1.,0.));
#6987=DIRECTION('ref_axis',(1.,0.,0.));
#6988=DIRECTION('center_axis',(0.,-1.,0.));
#6989=DIRECTION('ref_axis',(1.,0.,0.));
#6990=DIRECTION('center_axis',(0.,1.,0.));
#6991=DIRECTION('ref_axis',(1.,0.,0.));
#6992=DIRECTION('',(0.,-1.,0.));
#6993=DIRECTION('center_axis',(0.,1.,0.));
#6994=DIRECTION('ref_axis',(1.,0.,0.));
#6995=DIRECTION('center_axis',(0.,1.,0.));
#6996=DIRECTION('ref_axis',(1.,0.,0.));
#6997=DIRECTION('',(0.,-1.,0.));
#6998=DIRECTION('center_axis',(0.,1.,0.));
#6999=DIRECTION('ref_axis',(1.,0.,0.));
#7000=DIRECTION('center_axis',(0.,1.,0.));
#7001=DIRECTION('ref_axis',(1.,0.,0.));
#7002=DIRECTION('center_axis',(0.,1.,0.));
#7003=DIRECTION('ref_axis',(1.,0.,0.));
#7004=DIRECTION('axis',(0.,0.,1.));
#7005=DIRECTION('refdir',(1.,0.,0.));
#7006=DIRECTION('center_axis',(1.,0.,0.));
#7007=DIRECTION('ref_axis',(0.,0.,-1.));
#7008=DIRECTION('center_axis',(1.,0.,0.));
#7009=DIRECTION('ref_axis',(0.,0.,-1.));
#7010=DIRECTION('',(1.,0.,0.));
#7011=DIRECTION('center_axis',(-1.,0.,0.));
#7012=DIRECTION('ref_axis',(0.,0.,-1.));
#7013=DIRECTION('center_axis',(1.,0.,0.));
#7014=DIRECTION('ref_axis',(0.,0.,-1.));
#7015=DIRECTION('center_axis',(1.,0.,0.));
#7016=DIRECTION('ref_axis',(0.,0.,-1.));
#7017=DIRECTION('',(1.,0.,0.));
#7018=DIRECTION('center_axis',(-1.,0.,0.));
#7019=DIRECTION('ref_axis',(0.,0.,-1.));
#7020=DIRECTION('center_axis',(1.,0.,0.));
#7021=DIRECTION('ref_axis',(0.,0.,-1.));
#7022=DIRECTION('center_axis',(1.,0.,0.));
#7023=DIRECTION('ref_axis',(0.,0.,-1.));
#7024=DIRECTION('',(1.,0.,0.));
#7025=DIRECTION('center_axis',(-1.,0.,0.));
#7026=DIRECTION('ref_axis',(0.,0.,-1.));
#7027=DIRECTION('center_axis',(1.,0.,0.));
#7028=DIRECTION('ref_axis',(0.,0.,-1.));
#7029=DIRECTION('center_axis',(1.,0.,0.));
#7030=DIRECTION('ref_axis',(0.,0.,-1.));
#7031=DIRECTION('',(1.,0.,0.));
#7032=DIRECTION('center_axis',(-1.,0.,0.));
#7033=DIRECTION('ref_axis',(0.,0.,-1.));
#7034=DIRECTION('center_axis',(1.,0.,0.));
#7035=DIRECTION('ref_axis',(0.,0.,-1.));
#7036=DIRECTION('center_axis',(1.,0.,0.));
#7037=DIRECTION('ref_axis',(0.,0.,-1.));
#7038=DIRECTION('',(1.,0.,0.));
#7039=DIRECTION('center_axis',(-1.,0.,0.));
#7040=DIRECTION('ref_axis',(0.,0.,-1.));
#7041=DIRECTION('center_axis',(1.,0.,0.));
#7042=DIRECTION('ref_axis',(0.,0.,-1.));
#7043=DIRECTION('center_axis',(1.,0.,0.));
#7044=DIRECTION('ref_axis',(0.,0.,-1.));
#7045=DIRECTION('',(-1.,0.,0.));
#7046=DIRECTION('center_axis',(-1.,0.,0.));
#7047=DIRECTION('ref_axis',(0.,0.,-1.));
#7048=DIRECTION('center_axis',(1.,0.,0.));
#7049=DIRECTION('ref_axis',(0.,0.,-1.));
#7050=DIRECTION('center_axis',(0.,0.,1.));
#7051=DIRECTION('ref_axis',(1.,0.,0.));
#7052=DIRECTION('center_axis',(0.,0.,1.));
#7053=DIRECTION('ref_axis',(1.,0.,0.));
#7054=DIRECTION('',(0.,0.,1.));
#7055=DIRECTION('center_axis',(0.,0.,-1.));
#7056=DIRECTION('ref_axis',(1.,0.,0.));
#7057=DIRECTION('center_axis',(0.,0.,1.));
#7058=DIRECTION('ref_axis',(1.,0.,0.));
#7059=DIRECTION('center_axis',(0.,0.,1.));
#7060=DIRECTION('ref_axis',(1.,0.,0.));
#7061=DIRECTION('center_axis',(0.,0.,1.));
#7062=DIRECTION('ref_axis',(1.,0.,0.));
#7063=DIRECTION('',(0.,0.,1.));
#7064=DIRECTION('center_axis',(0.,0.,-1.));
#7065=DIRECTION('ref_axis',(1.,0.,0.));
#7066=DIRECTION('center_axis',(0.,0.,-1.));
#7067=DIRECTION('ref_axis',(-1.,0.,0.));
#7068=DIRECTION('',(0.,-1.,0.));
#7069=DIRECTION('',(1.,0.,0.));
#7070=DIRECTION('',(0.,1.,0.));
#7071=DIRECTION('',(-1.,0.,0.));
#7072=DIRECTION('center_axis',(0.,0.,1.));
#7073=DIRECTION('ref_axis',(1.,0.,0.));
#7074=DIRECTION('',(0.,1.,0.));
#7075=DIRECTION('',(1.,0.,0.));
#7076=DIRECTION('',(0.,-1.,0.));
#7077=DIRECTION('',(-1.,0.,0.));
#7078=DIRECTION('center_axis',(0.,1.,0.));
#7079=DIRECTION('ref_axis',(0.,0.,1.));
#7080=DIRECTION('',(0.,0.,-1.));
#7081=DIRECTION('',(-1.,0.,0.));
#7082=DIRECTION('',(0.,0.,-1.));
#7083=DIRECTION('',(1.,0.,0.));
#7084=DIRECTION('',(0.,0.,-1.));
#7085=DIRECTION('center_axis',(0.,-1.,0.));
#7086=DIRECTION('ref_axis',(1.,0.,0.));
#7087=DIRECTION('center_axis',(0.,1.,0.));
#7088=DIRECTION('ref_axis',(-1.,0.,-1.22464679914735E-16));
#7089=DIRECTION('center_axis',(0.,1.,0.));
#7090=DIRECTION('ref_axis',(1.,0.,0.));
#7091=DIRECTION('center_axis',(1.,0.,0.));
#7092=DIRECTION('ref_axis',(0.,0.,-1.));
#7093=DIRECTION('',(0.,1.,0.));
#7094=DIRECTION('',(0.,0.,1.));
#7095=DIRECTION('center_axis',(0.,0.,-1.));
#7096=DIRECTION('ref_axis',(-1.,0.,0.));
#7097=DIRECTION('',(1.,0.,0.));
#7098=DIRECTION('',(0.,-1.,0.));
#7099=DIRECTION('',(0.,1.,0.));
#7100=DIRECTION('center_axis',(1.,0.,0.));
#7101=DIRECTION('ref_axis',(0.,0.,-1.));
#7102=DIRECTION('',(0.,0.,1.));
#7103=DIRECTION('center_axis',(0.,0.,1.));
#7104=DIRECTION('ref_axis',(1.,0.,0.));
#7105=DIRECTION('',(-1.,0.,0.));
#7106=DIRECTION('',(0.,1.,0.));
#7107=DIRECTION('center_axis',(0.,1.,0.));
#7108=DIRECTION('ref_axis',(1.,0.,0.));
#7109=DIRECTION('',(0.,0.,1.));
#7110=DIRECTION('center_axis',(0.,0.,1.));
#7111=DIRECTION('ref_axis',(1.,0.,0.));
#7112=DIRECTION('center_axis',(0.,0.,1.));
#7113=DIRECTION('ref_axis',(1.,0.,0.));
#7114=DIRECTION('',(0.,0.,1.));
#7115=DIRECTION('center_axis',(0.,0.,-1.));
#7116=DIRECTION('ref_axis',(1.,0.,0.));
#7117=DIRECTION('center_axis',(0.,0.,1.));
#7118=DIRECTION('ref_axis',(1.,0.,0.));
#7119=DIRECTION('center_axis',(0.,0.,1.));
#7120=DIRECTION('ref_axis',(1.,0.,0.));
#7121=DIRECTION('center_axis',(0.,0.,1.));
#7122=DIRECTION('ref_axis',(1.,0.,0.));
#7123=DIRECTION('',(0.,0.,1.));
#7124=DIRECTION('center_axis',(0.,0.,-1.));
#7125=DIRECTION('ref_axis',(1.,0.,0.));
#7126=DIRECTION('center_axis',(0.,0.,-1.));
#7127=DIRECTION('ref_axis',(-1.,0.,0.));
#7128=DIRECTION('',(0.,-1.,0.));
#7129=DIRECTION('',(1.,0.,0.));
#7130=DIRECTION('',(0.,1.,0.));
#7131=DIRECTION('',(-1.,0.,0.));
#7132=DIRECTION('center_axis',(0.,0.,1.));
#7133=DIRECTION('ref_axis',(1.,0.,0.));
#7134=DIRECTION('',(0.,1.,0.));
#7135=DIRECTION('',(1.,0.,0.));
#7136=DIRECTION('',(0.,-1.,0.));
#7137=DIRECTION('',(-1.,0.,0.));
#7138=DIRECTION('center_axis',(0.,1.,0.));
#7139=DIRECTION('ref_axis',(0.,0.,1.));
#7140=DIRECTION('',(0.,0.,-1.));
#7141=DIRECTION('',(-1.,0.,0.));
#7142=DIRECTION('',(0.,0.,-1.));
#7143=DIRECTION('',(1.,0.,0.));
#7144=DIRECTION('',(0.,0.,-1.));
#7145=DIRECTION('center_axis',(0.,-1.,0.));
#7146=DIRECTION('ref_axis',(1.,0.,0.));
#7147=DIRECTION('center_axis',(0.,1.,0.));
#7148=DIRECTION('ref_axis',(-1.,0.,-1.22464679914735E-16));
#7149=DIRECTION('center_axis',(0.,1.,0.));
#7150=DIRECTION('ref_axis',(1.,0.,0.));
#7151=DIRECTION('center_axis',(1.,0.,0.));
#7152=DIRECTION('ref_axis',(0.,0.,-1.));
#7153=DIRECTION('',(0.,1.,0.));
#7154=DIRECTION('',(0.,0.,1.));
#7155=DIRECTION('center_axis',(0.,0.,-1.));
#7156=DIRECTION('ref_axis',(-1.,0.,0.));
#7157=DIRECTION('',(1.,0.,0.));
#7158=DIRECTION('',(0.,-1.,0.));
#7159=DIRECTION('',(0.,1.,0.));
#7160=DIRECTION('center_axis',(1.,0.,0.));
#7161=DIRECTION('ref_axis',(0.,0.,-1.));
#7162=DIRECTION('',(0.,0.,1.));
#7163=DIRECTION('center_axis',(0.,0.,1.));
#7164=DIRECTION('ref_axis',(1.,0.,0.));
#7165=DIRECTION('',(-1.,0.,0.));
#7166=DIRECTION('',(0.,1.,0.));
#7167=DIRECTION('center_axis',(0.,1.,0.));
#7168=DIRECTION('ref_axis',(1.,0.,0.));
#7169=DIRECTION('',(0.,0.,1.));
#7170=DIRECTION('center_axis',(0.,1.,0.));
#7171=DIRECTION('ref_axis',(-1.,0.,0.));
#7172=DIRECTION('',(-1.,0.,0.));
#7173=DIRECTION('',(0.,0.,1.));
#7174=DIRECTION('',(-1.,0.,0.));
#7175=DIRECTION('',(0.,0.,1.));
#7176=DIRECTION('center_axis',(1.,0.,0.));
#7177=DIRECTION('ref_axis',(0.,1.,0.));
#7178=DIRECTION('',(0.,1.,0.));
#7179=DIRECTION('',(0.,1.,0.));
#7180=DIRECTION('',(0.,0.,1.));
#7181=DIRECTION('center_axis',(0.,-1.,0.));
#7182=DIRECTION('ref_axis',(1.,0.,0.));
#7183=DIRECTION('',(1.,0.,0.));
#7184=DIRECTION('',(1.,0.,0.));
#7185=DIRECTION('',(0.,0.,1.));
#7186=DIRECTION('center_axis',(-1.,0.,0.));
#7187=DIRECTION('ref_axis',(0.,-1.,0.));
#7188=DIRECTION('',(0.,-1.,0.));
#7189=DIRECTION('',(0.,-1.,0.));
#7190=DIRECTION('center_axis',(0.,0.,1.));
#7191=DIRECTION('ref_axis',(1.,0.,0.));
#7192=DIRECTION('center_axis',(0.,0.,1.));
#7193=DIRECTION('ref_axis',(1.,0.,0.));
#7194=DIRECTION('axis',(0.,0.,1.));
#7195=DIRECTION('refdir',(1.,0.,0.));
#7196=DIRECTION('center_axis',(1.,0.,0.));
#7197=DIRECTION('ref_axis',(0.,0.,-1.));
#7198=DIRECTION('center_axis',(1.,0.,0.));
#7199=DIRECTION('ref_axis',(0.,0.,-1.));
#7200=DIRECTION('',(1.,0.,0.));
#7201=DIRECTION('center_axis',(-1.,0.,0.));
#7202=DIRECTION('ref_axis',(0.,0.,-1.));
#7203=DIRECTION('center_axis',(0.,0.,-1.));
#7204=DIRECTION('ref_axis',(0.,1.,0.));
#7205=DIRECTION('',(0.,1.,0.));
#7206=DIRECTION('',(1.,0.,0.));
#7207=DIRECTION('',(0.,1.,0.));
#7208=DIRECTION('',(1.,0.,0.));
#7209=DIRECTION('center_axis',(0.,-0.866025403784439,-0.499999999999999));
#7210=DIRECTION('ref_axis',(0.,0.499999999999999,-0.866025403784439));
#7211=DIRECTION('',(0.,0.499999999999999,-0.866025403784439));
#7212=DIRECTION('',(0.,0.499999999999999,-0.866025403784439));
#7213=DIRECTION('',(1.,0.,0.));
#7214=DIRECTION('center_axis',(0.,-0.866025403784439,0.499999999999999));
#7215=DIRECTION('ref_axis',(0.,-0.499999999999999,-0.866025403784439));
#7216=DIRECTION('',(0.,-0.499999999999999,-0.866025403784439));
#7217=DIRECTION('',(0.,-0.499999999999999,-0.866025403784439));
#7218=DIRECTION('',(1.,0.,0.));
#7219=DIRECTION('center_axis',(0.,0.,1.));
#7220=DIRECTION('ref_axis',(0.,-1.,0.));
#7221=DIRECTION('',(0.,-1.,0.));
#7222=DIRECTION('',(0.,-1.,0.));
#7223=DIRECTION('',(1.,0.,0.));
#7224=DIRECTION('center_axis',(0.,0.866025403784439,0.499999999999999));
#7225=DIRECTION('ref_axis',(0.,-0.499999999999999,0.866025403784439));
#7226=DIRECTION('',(0.,-0.499999999999999,0.866025403784439));
#7227=DIRECTION('',(0.,-0.499999999999999,0.866025403784439));
#7228=DIRECTION('',(1.,0.,0.));
#7229=DIRECTION('center_axis',(0.,0.866025403784439,-0.499999999999999));
#7230=DIRECTION('ref_axis',(0.,0.499999999999999,0.866025403784439));
#7231=DIRECTION('',(0.,0.499999999999999,0.866025403784439));
#7232=DIRECTION('',(0.,0.499999999999999,0.866025403784439));
#7233=DIRECTION('center_axis',(1.,0.,0.));
#7234=DIRECTION('ref_axis',(0.,0.,-1.));
#7235=DIRECTION('center_axis',(1.,0.,0.));
#7236=DIRECTION('ref_axis',(0.,0.,-1.));
#7237=DIRECTION('axis',(0.,0.,1.));
#7238=DIRECTION('refdir',(1.,0.,0.));
#7239=DIRECTION('center_axis',(0.,1.,0.));
#7240=DIRECTION('ref_axis',(0.,0.,1.));
#7241=DIRECTION('center_axis',(0.,-1.,0.));
#7242=DIRECTION('ref_axis',(1.,0.,0.));
#7243=DIRECTION('center_axis',(0.,-1.,0.));
#7244=DIRECTION('ref_axis',(1.,0.,0.));
#7245=DIRECTION('center_axis',(0.,-1.,0.));
#7246=DIRECTION('ref_axis',(1.,0.,0.));
#7247=DIRECTION('center_axis',(0.,-1.,0.));
#7248=DIRECTION('ref_axis',(1.,0.,0.));
#7249=DIRECTION('',(0.0747899482416342,0.997199309888456,9.15912707225136E-18));
#7250=DIRECTION('center_axis',(0.,-1.,0.));
#7251=DIRECTION('ref_axis',(0.,0.,-1.));
#7252=DIRECTION('center_axis',(0.,-1.,0.));
#7253=DIRECTION('ref_axis',(1.,0.,0.));
#7254=DIRECTION('center_axis',(0.,-1.,0.));
#7255=DIRECTION('ref_axis',(1.,0.,0.));
#7256=DIRECTION('center_axis',(0.,-1.,0.));
#7257=DIRECTION('ref_axis',(1.,0.,0.));
#7258=DIRECTION('',(0.,1.,0.));
#7259=DIRECTION('center_axis',(0.,-1.,0.));
#7260=DIRECTION('ref_axis',(1.,0.,0.));
#7261=DIRECTION('center_axis',(0.,-1.,0.));
#7262=DIRECTION('ref_axis',(1.,0.,0.));
#7263=DIRECTION('',(0.0747899482416342,0.997199309888456,9.15912707225136E-18));
#7264=DIRECTION('center_axis',(0.,-1.,0.));
#7265=DIRECTION('ref_axis',(0.,0.,-1.));
#7266=DIRECTION('center_axis',(0.,-1.,0.));
#7267=DIRECTION('ref_axis',(1.,0.,0.));
#7268=DIRECTION('center_axis',(0.,-1.,0.));
#7269=DIRECTION('ref_axis',(1.,0.,0.));
#7270=DIRECTION('center_axis',(0.,-1.,0.));
#7271=DIRECTION('ref_axis',(1.,0.,0.));
#7272=DIRECTION('',(0.,1.,0.));
#7273=DIRECTION('center_axis',(0.,-1.,0.));
#7274=DIRECTION('ref_axis',(1.,0.,0.));
#7275=DIRECTION('center_axis',(0.,-1.,0.));
#7276=DIRECTION('ref_axis',(1.,0.,0.));
#7277=DIRECTION('',(0.0747899482416342,0.997199309888456,9.15912707225136E-18));
#7278=DIRECTION('center_axis',(0.,-1.,0.));
#7279=DIRECTION('ref_axis',(0.,0.,-1.));
#7280=DIRECTION('center_axis',(0.,-1.,0.));
#7281=DIRECTION('ref_axis',(1.,0.,0.));
#7282=DIRECTION('center_axis',(0.,-1.,0.));
#7283=DIRECTION('ref_axis',(1.,0.,0.));
#7284=DIRECTION('center_axis',(0.,-1.,0.));
#7285=DIRECTION('ref_axis',(1.,0.,0.));
#7286=DIRECTION('',(0.,1.,0.));
#7287=DIRECTION('center_axis',(0.,-1.,0.));
#7288=DIRECTION('ref_axis',(1.,0.,0.));
#7289=DIRECTION('center_axis',(0.,-1.,0.));
#7290=DIRECTION('ref_axis',(1.,0.,0.));
#7291=DIRECTION('',(0.,1.,0.));
#7292=DIRECTION('center_axis',(0.,1.,0.));
#7293=DIRECTION('ref_axis',(1.,0.,0.));
#7294=DIRECTION('',(1.,0.,0.));
#7295=DIRECTION('',(0.5,0.,0.866025403784439));
#7296=DIRECTION('',(-0.5,0.,0.866025403784439));
#7297=DIRECTION('',(-1.,0.,0.));
#7298=DIRECTION('',(-0.5,0.,-0.866025403784439));
#7299=DIRECTION('',(0.5,0.,-0.866025403784439));
#7300=DIRECTION('center_axis',(0.,1.,0.));
#7301=DIRECTION('ref_axis',(1.,0.,0.));
#7302=DIRECTION('center_axis',(0.866025403784439,0.,-0.5));
#7303=DIRECTION('ref_axis',(-0.5,0.,-0.866025403784439));
#7304=DIRECTION('',(0.,1.,0.));
#7305=DIRECTION('',(-0.5,0.,-0.866025403784439));
#7306=DIRECTION('',(0.,1.,0.));
#7307=DIRECTION('center_axis',(0.866025403784439,0.,0.5));
#7308=DIRECTION('ref_axis',(0.5,0.,-0.866025403784439));
#7309=DIRECTION('',(0.5,0.,-0.866025403784439));
#7310=DIRECTION('',(0.,1.,0.));
#7311=DIRECTION('center_axis',(0.,0.,1.));
#7312=DIRECTION('ref_axis',(1.,0.,0.));
#7313=DIRECTION('',(1.,0.,0.));
#7314=DIRECTION('',(0.,1.,0.));
#7315=DIRECTION('center_axis',(-0.866025403784439,0.,0.5));
#7316=DIRECTION('ref_axis',(0.5,0.,0.866025403784439));
#7317=DIRECTION('',(0.5,0.,0.866025403784439));
#7318=DIRECTION('',(0.,1.,0.));
#7319=DIRECTION('center_axis',(-0.866025403784439,0.,-0.5));
#7320=DIRECTION('ref_axis',(-0.5,0.,0.866025403784439));
#7321=DIRECTION('',(-0.5,0.,0.866025403784439));
#7322=DIRECTION('',(0.,1.,0.));
#7323=DIRECTION('center_axis',(0.,0.,-1.));
#7324=DIRECTION('ref_axis',(-1.,0.,0.));
#7325=DIRECTION('',(-1.,0.,0.));
#7326=DIRECTION('center_axis',(0.,1.,0.));
#7327=DIRECTION('ref_axis',(0.,0.,1.));
#7328=DIRECTION('center_axis',(0.,1.,0.));
#7329=DIRECTION('ref_axis',(1.,0.,0.));
#7330=DIRECTION('',(0.,-1.,0.));
#7331=DIRECTION('center_axis',(0.,1.,0.));
#7332=DIRECTION('ref_axis',(1.,0.,0.));
#7333=DIRECTION('center_axis',(0.,1.,0.));
#7334=DIRECTION('ref_axis',(1.,0.,0.));
#7335=DIRECTION('axis',(0.,0.,1.));
#7336=DIRECTION('refdir',(1.,0.,0.));
#7337=DIRECTION('center_axis',(0.,0.,1.));
#7338=DIRECTION('ref_axis',(1.,0.,0.));
#7339=DIRECTION('center_axis',(0.,0.,1.));
#7340=DIRECTION('ref_axis',(1.,0.,0.));
#7341=DIRECTION('',(0.,0.,1.));
#7342=DIRECTION('center_axis',(0.,0.,-1.));
#7343=DIRECTION('ref_axis',(1.,0.,0.));
#7344=DIRECTION('center_axis',(0.,0.,1.));
#7345=DIRECTION('ref_axis',(1.,0.,0.));
#7346=DIRECTION('center_axis',(0.,0.,1.));
#7347=DIRECTION('ref_axis',(1.,0.,0.));
#7348=DIRECTION('center_axis',(0.,0.,1.));
#7349=DIRECTION('ref_axis',(1.,0.,0.));
#7350=DIRECTION('',(0.,0.,1.));
#7351=DIRECTION('center_axis',(0.,0.,-1.));
#7352=DIRECTION('ref_axis',(1.,0.,0.));
#7353=DIRECTION('center_axis',(0.,0.,1.));
#7354=DIRECTION('ref_axis',(1.,0.,0.));
#7355=DIRECTION('center_axis',(0.,1.,0.));
#7356=DIRECTION('ref_axis',(1.,0.,0.));
#7357=DIRECTION('center_axis',(0.,1.,0.));
#7358=DIRECTION('ref_axis',(1.,0.,0.));
#7359=DIRECTION('',(0.,1.,0.));
#7360=DIRECTION('center_axis',(0.,-1.,0.));
#7361=DIRECTION('ref_axis',(1.,0.,0.));
#7362=DIRECTION('center_axis',(0.,1.,0.));
#7363=DIRECTION('ref_axis',(1.,0.,0.));
#7364=DIRECTION('center_axis',(0.,1.,0.));
#7365=DIRECTION('ref_axis',(1.,0.,0.));
#7366=DIRECTION('',(0.,1.,0.));
#7367=DIRECTION('center_axis',(0.,-1.,0.));
#7368=DIRECTION('ref_axis',(1.,0.,0.));
#7369=DIRECTION('center_axis',(0.,1.,0.));
#7370=DIRECTION('ref_axis',(1.,0.,0.));
#7371=DIRECTION('center_axis',(0.,1.,0.));
#7372=DIRECTION('ref_axis',(1.,0.,0.));
#7373=DIRECTION('',(0.,1.,0.));
#7374=DIRECTION('center_axis',(0.,-1.,0.));
#7375=DIRECTION('ref_axis',(1.,0.,0.));
#7376=DIRECTION('center_axis',(0.,1.,0.));
#7377=DIRECTION('ref_axis',(1.,0.,0.));
#7378=DIRECTION('center_axis',(0.,1.,0.));
#7379=DIRECTION('ref_axis',(1.,0.,0.));
#7380=DIRECTION('',(0.,1.,0.));
#7381=DIRECTION('center_axis',(0.,-1.,0.));
#7382=DIRECTION('ref_axis',(1.,0.,0.));
#7383=DIRECTION('center_axis',(0.,0.,1.));
#7384=DIRECTION('ref_axis',(1.,0.,0.));
#7385=DIRECTION('',(0.,0.,1.));
#7386=DIRECTION('center_axis',(0.,0.,1.));
#7387=DIRECTION('ref_axis',(1.,0.,0.));
#7388=DIRECTION('',(0.,0.,-1.));
#7389=DIRECTION('center_axis',(0.,0.,-1.));
#7390=DIRECTION('ref_axis',(1.,0.,0.));
#7391=DIRECTION('center_axis',(0.,0.,1.));
#7392=DIRECTION('ref_axis',(1.,0.,0.));
#7393=DIRECTION('',(1.,0.,0.));
#7394=DIRECTION('center_axis',(0.,0.,1.));
#7395=DIRECTION('ref_axis',(0.,-1.,0.));
#7396=DIRECTION('',(1.,0.,0.));
#7397=DIRECTION('center_axis',(0.,0.,1.));
#7398=DIRECTION('ref_axis',(1.,0.,0.));
#7399=DIRECTION('',(-1.,0.,0.));
#7400=DIRECTION('',(0.,-1.,0.));
#7401=DIRECTION('',(1.,0.,0.));
#7402=DIRECTION('',(0.,1.,0.));
#7403=DIRECTION('',(-1.,0.,0.));
#7404=DIRECTION('center_axis',(0.,1.,0.));
#7405=DIRECTION('ref_axis',(1.,0.,0.));
#7406=DIRECTION('center_axis',(0.,1.,0.));
#7407=DIRECTION('ref_axis',(1.,0.,0.));
#7408=DIRECTION('',(0.,1.,0.));
#7409=DIRECTION('center_axis',(0.,-1.,0.));
#7410=DIRECTION('ref_axis',(1.,0.,0.));
#7411=DIRECTION('center_axis',(0.,1.,0.));
#7412=DIRECTION('ref_axis',(1.,0.,0.));
#7413=DIRECTION('center_axis',(0.,1.,0.));
#7414=DIRECTION('ref_axis',(1.,0.,0.));
#7415=DIRECTION('',(0.,1.,0.));
#7416=DIRECTION('center_axis',(0.,1.,0.));
#7417=DIRECTION('ref_axis',(1.,0.,0.));
#7418=DIRECTION('center_axis',(0.,1.,0.));
#7419=DIRECTION('ref_axis',(1.,0.,0.));
#7420=DIRECTION('center_axis',(0.,-1.,0.));
#7421=DIRECTION('ref_axis',(0.,0.,-1.));
#7422=DIRECTION('center_axis',(0.,1.,0.));
#7423=DIRECTION('ref_axis',(1.,0.,0.));
#7424=DIRECTION('center_axis',(6.12323399573677E-17,0.,1.));
#7425=DIRECTION('ref_axis',(1.,0.,0.));
#7426=DIRECTION('center_axis',(0.,-1.,0.));
#7427=DIRECTION('ref_axis',(0.,0.,-1.));
#7428=DIRECTION('center_axis',(0.,1.,0.));
#7429=DIRECTION('ref_axis',(-1.,0.,0.));
#7430=DIRECTION('',(0.,0.,1.));
#7431=DIRECTION('',(-1.,0.,0.));
#7432=DIRECTION('',(0.,0.,1.));
#7433=DIRECTION('center_axis',(1.,0.,0.));
#7434=DIRECTION('ref_axis',(0.,1.,0.));
#7435=DIRECTION('',(0.,1.,0.));
#7436=DIRECTION('',(0.,0.,1.));
#7437=DIRECTION('center_axis',(0.,-1.,0.));
#7438=DIRECTION('ref_axis',(1.,0.,0.));
#7439=DIRECTION('',(1.,0.,0.));
#7440=DIRECTION('',(0.,0.,1.));
#7441=DIRECTION('center_axis',(-1.,0.,0.));
#7442=DIRECTION('ref_axis',(0.,-1.,0.));
#7443=DIRECTION('',(0.,-1.,0.));
#7444=DIRECTION('center_axis',(0.,0.,1.));
#7445=DIRECTION('ref_axis',(1.,0.,0.));
#7446=DIRECTION('axis',(0.,0.,1.));
#7447=DIRECTION('refdir',(1.,0.,0.));
#7448=DIRECTION('center_axis',(0.,0.,1.));
#7449=DIRECTION('ref_axis',(1.,0.,0.));
#7450=DIRECTION('center_axis',(0.,0.,1.));
#7451=DIRECTION('ref_axis',(1.,0.,0.));
#7452=DIRECTION('',(0.,0.,1.));
#7453=DIRECTION('center_axis',(0.,0.,-1.));
#7454=DIRECTION('ref_axis',(1.,0.,0.));
#7455=DIRECTION('center_axis',(0.,0.,1.));
#7456=DIRECTION('ref_axis',(1.,0.,0.));
#7457=DIRECTION('center_axis',(0.,0.,1.));
#7458=DIRECTION('ref_axis',(1.,0.,0.));
#7459=DIRECTION('center_axis',(0.,0.,1.));
#7460=DIRECTION('ref_axis',(1.,0.,0.));
#7461=DIRECTION('',(0.,0.,1.));
#7462=DIRECTION('center_axis',(0.,0.,-1.));
#7463=DIRECTION('ref_axis',(1.,0.,0.));
#7464=DIRECTION('center_axis',(0.,0.,1.));
#7465=DIRECTION('ref_axis',(1.,0.,0.));
#7466=DIRECTION('center_axis',(0.,1.,0.));
#7467=DIRECTION('ref_axis',(1.,0.,0.));
#7468=DIRECTION('center_axis',(0.,1.,0.));
#7469=DIRECTION('ref_axis',(1.,0.,0.));
#7470=DIRECTION('',(0.,1.,0.));
#7471=DIRECTION('center_axis',(0.,-1.,0.));
#7472=DIRECTION('ref_axis',(1.,0.,0.));
#7473=DIRECTION('center_axis',(0.,1.,0.));
#7474=DIRECTION('ref_axis',(1.,0.,0.));
#7475=DIRECTION('center_axis',(0.,1.,0.));
#7476=DIRECTION('ref_axis',(1.,0.,0.));
#7477=DIRECTION('',(0.,1.,0.));
#7478=DIRECTION('center_axis',(0.,-1.,0.));
#7479=DIRECTION('ref_axis',(1.,0.,0.));
#7480=DIRECTION('center_axis',(0.,1.,0.));
#7481=DIRECTION('ref_axis',(1.,0.,0.));
#7482=DIRECTION('center_axis',(0.,1.,0.));
#7483=DIRECTION('ref_axis',(1.,0.,0.));
#7484=DIRECTION('',(0.,1.,0.));
#7485=DIRECTION('center_axis',(0.,-1.,0.));
#7486=DIRECTION('ref_axis',(1.,0.,0.));
#7487=DIRECTION('center_axis',(0.,1.,0.));
#7488=DIRECTION('ref_axis',(1.,0.,0.));
#7489=DIRECTION('center_axis',(0.,1.,0.));
#7490=DIRECTION('ref_axis',(1.,0.,0.));
#7491=DIRECTION('',(0.,1.,0.));
#7492=DIRECTION('center_axis',(0.,-1.,0.));
#7493=DIRECTION('ref_axis',(1.,0.,0.));
#7494=DIRECTION('center_axis',(0.,0.,1.));
#7495=DIRECTION('ref_axis',(1.,0.,0.));
#7496=DIRECTION('',(0.,0.,1.));
#7497=DIRECTION('center_axis',(0.,0.,1.));
#7498=DIRECTION('ref_axis',(1.,0.,0.));
#7499=DIRECTION('',(0.,0.,-1.));
#7500=DIRECTION('center_axis',(0.,0.,-1.));
#7501=DIRECTION('ref_axis',(1.,0.,0.));
#7502=DIRECTION('center_axis',(0.,0.,1.));
#7503=DIRECTION('ref_axis',(1.,0.,0.));
#7504=DIRECTION('',(-1.,0.,0.));
#7505=DIRECTION('center_axis',(0.,0.,1.));
#7506=DIRECTION('ref_axis',(0.,-1.,0.));
#7507=DIRECTION('',(-1.,0.,0.));
#7508=DIRECTION('center_axis',(0.,0.,1.));
#7509=DIRECTION('ref_axis',(1.,0.,0.));
#7510=DIRECTION('',(1.,0.,0.));
#7511=DIRECTION('',(0.,1.,0.));
#7512=DIRECTION('',(-1.,0.,0.));
#7513=DIRECTION('',(0.,-1.,0.));
#7514=DIRECTION('',(1.,0.,0.));
#7515=DIRECTION('center_axis',(0.,1.,0.));
#7516=DIRECTION('ref_axis',(1.,0.,0.));
#7517=DIRECTION('center_axis',(0.,1.,0.));
#7518=DIRECTION('ref_axis',(1.,0.,0.));
#7519=DIRECTION('',(0.,1.,0.));
#7520=DIRECTION('center_axis',(0.,-1.,0.));
#7521=DIRECTION('ref_axis',(1.,0.,0.));
#7522=DIRECTION('center_axis',(0.,1.,0.));
#7523=DIRECTION('ref_axis',(1.,0.,0.));
#7524=DIRECTION('center_axis',(0.,1.,0.));
#7525=DIRECTION('ref_axis',(1.,0.,0.));
#7526=DIRECTION('',(0.,1.,0.));
#7527=DIRECTION('center_axis',(0.,1.,0.));
#7528=DIRECTION('ref_axis',(1.,0.,0.));
#7529=DIRECTION('center_axis',(0.,1.,0.));
#7530=DIRECTION('ref_axis',(1.,0.,0.));
#7531=DIRECTION('center_axis',(0.,1.,0.));
#7532=DIRECTION('ref_axis',(1.,0.,0.));
#7533=DIRECTION('center_axis',(0.,1.,0.));
#7534=DIRECTION('ref_axis',(0.,0.,1.));
#7535=DIRECTION('center_axis',(6.12323399573677E-17,0.,1.));
#7536=DIRECTION('ref_axis',(1.,0.,0.));
#7537=DIRECTION('center_axis',(0.,1.,0.));
#7538=DIRECTION('ref_axis',(0.,0.,1.));
#7539=DIRECTION('center_axis',(0.,1.,0.));
#7540=DIRECTION('ref_axis',(-1.,0.,0.));
#7541=DIRECTION('',(-1.,0.,0.));
#7542=DIRECTION('',(0.,0.,1.));
#7543=DIRECTION('',(0.,0.,1.));
#7544=DIRECTION('center_axis',(1.,0.,0.));
#7545=DIRECTION('ref_axis',(0.,1.,0.));
#7546=DIRECTION('',(0.,1.,0.));
#7547=DIRECTION('',(0.,0.,1.));
#7548=DIRECTION('center_axis',(0.,-1.,0.));
#7549=DIRECTION('ref_axis',(1.,0.,0.));
#7550=DIRECTION('',(0.,0.,1.));
#7551=DIRECTION('',(1.,0.,0.));
#7552=DIRECTION('center_axis',(-1.,0.,0.));
#7553=DIRECTION('ref_axis',(0.,-1.,0.));
#7554=DIRECTION('',(0.,-1.,0.));
#7555=DIRECTION('center_axis',(0.,0.,1.));
#7556=DIRECTION('ref_axis',(1.,0.,0.));
#7557=DIRECTION('axis',(0.,0.,1.));
#7558=DIRECTION('refdir',(1.,0.,0.));
#7559=DIRECTION('center_axis',(0.,1.,0.));
#7560=DIRECTION('ref_axis',(1.,0.,0.));
#7561=DIRECTION('center_axis',(0.,1.,0.));
#7562=DIRECTION('ref_axis',(1.,0.,0.));
#7563=DIRECTION('',(0.,1.,0.));
#7564=DIRECTION('center_axis',(0.,-1.,0.));
#7565=DIRECTION('ref_axis',(1.,0.,0.));
#7566=DIRECTION('center_axis',(0.,1.,0.));
#7567=DIRECTION('ref_axis',(1.,0.,0.));
#7568=DIRECTION('center_axis',(0.,1.,0.));
#7569=DIRECTION('ref_axis',(1.,0.,0.));
#7570=DIRECTION('',(0.,1.,0.));
#7571=DIRECTION('center_axis',(0.,-1.,0.));
#7572=DIRECTION('ref_axis',(1.,0.,0.));
#7573=DIRECTION('center_axis',(0.,1.,0.));
#7574=DIRECTION('ref_axis',(1.,0.,0.));
#7575=DIRECTION('center_axis',(0.,1.,0.));
#7576=DIRECTION('ref_axis',(1.,0.,0.));
#7577=DIRECTION('',(0.,1.,0.));
#7578=DIRECTION('center_axis',(0.,-1.,0.));
#7579=DIRECTION('ref_axis',(1.,0.,0.));
#7580=DIRECTION('center_axis',(0.,1.,0.));
#7581=DIRECTION('ref_axis',(1.,0.,0.));
#7582=DIRECTION('center_axis',(0.,1.,0.));
#7583=DIRECTION('ref_axis',(1.,0.,0.));
#7584=DIRECTION('',(0.,1.,0.));
#7585=DIRECTION('center_axis',(0.,-1.,0.));
#7586=DIRECTION('ref_axis',(1.,0.,0.));
#7587=DIRECTION('center_axis',(-1.,0.,0.));
#7588=DIRECTION('ref_axis',(0.,0.,1.));
#7589=DIRECTION('',(0.,0.,1.));
#7590=DIRECTION('',(0.,1.,0.));
#7591=DIRECTION('',(0.,0.,-1.));
#7592=DIRECTION('',(0.,1.,0.));
#7593=DIRECTION('center_axis',(0.,0.,-1.));
#7594=DIRECTION('ref_axis',(-1.,0.,0.));
#7595=DIRECTION('',(-1.,0.,0.));
#7596=DIRECTION('',(0.,1.,0.));
#7597=DIRECTION('',(1.,0.,0.));
#7598=DIRECTION('',(0.,1.,0.));
#7599=DIRECTION('center_axis',(0.,0.,-1.));
#7600=DIRECTION('ref_axis',(-1.,0.,0.));
#7601=DIRECTION('',(-1.,0.,0.));
#7602=DIRECTION('',(0.,-1.,0.));
#7603=DIRECTION('',(1.,0.,0.));
#7604=DIRECTION('center_axis',(1.,0.,0.));
#7605=DIRECTION('ref_axis',(0.,0.,-1.));
#7606=DIRECTION('',(0.,0.,-1.));
#7607=DIRECTION('',(0.,-1.,0.));
#7608=DIRECTION('',(0.,0.,1.));
#7609=DIRECTION('center_axis',(0.,1.,0.));
#7610=DIRECTION('ref_axis',(0.,0.,1.));
#7611=DIRECTION('center_axis',(0.,-1.,0.));
#7612=DIRECTION('ref_axis',(1.,0.,0.));
#7613=DIRECTION('',(1.,0.,0.));
#7614=DIRECTION('',(0.,0.,-1.));
#7615=DIRECTION('',(-1.,0.,0.));
#7616=DIRECTION('',(0.,0.,1.));
#7617=DIRECTION('',(1.,0.,0.));
#7618=DIRECTION('center_axis',(0.,0.,1.));
#7619=DIRECTION('ref_axis',(1.,0.,0.));
#7620=DIRECTION('',(-1.,0.,0.));
#7621=DIRECTION('',(0.,1.,0.));
#7622=DIRECTION('center_axis',(0.,0.,1.));
#7623=DIRECTION('ref_axis',(1.,0.,0.));
#7624=DIRECTION('',(0.,1.,0.));
#7625=DIRECTION('',(-1.,0.,0.));
#7626=DIRECTION('center_axis',(0.,1.,0.));
#7627=DIRECTION('ref_axis',(-1.83697019872103E-16,0.,-1.));
#7628=DIRECTION('center_axis',(0.,1.,0.));
#7629=DIRECTION('ref_axis',(1.,0.,0.));
#7630=DIRECTION('center_axis',(-1.,0.,0.));
#7631=DIRECTION('ref_axis',(0.,0.,1.));
#7632=DIRECTION('',(0.,0.,-1.));
#7633=DIRECTION('',(0.,1.,0.));
#7634=DIRECTION('center_axis',(0.,0.,-1.));
#7635=DIRECTION('ref_axis',(-1.,0.,0.));
#7636=DIRECTION('',(1.,0.,0.));
#7637=DIRECTION('',(0.,1.,0.));
#7638=DIRECTION('center_axis',(1.,0.,0.));
#7639=DIRECTION('ref_axis',(0.,0.,-1.));
#7640=DIRECTION('',(0.,0.,1.));
#7641=DIRECTION('center_axis',(0.,1.,0.));
#7642=DIRECTION('ref_axis',(1.,0.,0.));
#7643=DIRECTION('axis',(0.,0.,1.));
#7644=DIRECTION('refdir',(1.,0.,0.));
#7645=DIRECTION('center_axis',(0.,0.,1.));
#7646=DIRECTION('ref_axis',(1.,0.,0.));
#7647=DIRECTION('center_axis',(0.,0.,1.));
#7648=DIRECTION('ref_axis',(1.,0.,0.));
#7649=DIRECTION('center_axis',(0.,0.,1.));
#7650=DIRECTION('ref_axis',(1.,0.,0.));
#7651=DIRECTION('center_axis',(0.,0.,1.));
#7652=DIRECTION('ref_axis',(1.,0.,0.));
#7653=DIRECTION('center_axis',(0.,0.,1.));
#7654=DIRECTION('ref_axis',(1.,0.,0.));
#7655=DIRECTION('',(0.,0.,-1.));
#7656=DIRECTION('center_axis',(0.,0.,1.));
#7657=DIRECTION('ref_axis',(1.,0.,0.));
#7658=DIRECTION('center_axis',(0.,0.,-1.));
#7659=DIRECTION('ref_axis',(1.,0.,0.));
#7660=DIRECTION('center_axis',(0.,0.,1.));
#7661=DIRECTION('ref_axis',(1.,0.,0.));
#7662=DIRECTION('',(0.,0.,-1.));
#7663=DIRECTION('center_axis',(0.,0.,-1.));
#7664=DIRECTION('ref_axis',(1.,0.,0.));
#7665=DIRECTION('center_axis',(0.,0.,1.));
#7666=DIRECTION('ref_axis',(1.,0.,0.));
#7667=DIRECTION('',(0.,0.,-1.));
#7668=DIRECTION('center_axis',(0.,0.,1.));
#7669=DIRECTION('ref_axis',(1.,0.,0.));
#7670=DIRECTION('center_axis',(0.,0.,1.));
#7671=DIRECTION('ref_axis',(1.,0.,0.));
#7672=DIRECTION('axis',(0.,0.,1.));
#7673=DIRECTION('refdir',(1.,0.,0.));
#7674=DIRECTION('center_axis',(0.,0.,1.));
#7675=DIRECTION('ref_axis',(1.,0.,0.));
#7676=DIRECTION('center_axis',(1.22464679914735E-16,-1.,0.));
#7677=DIRECTION('ref_axis',(-1.,-1.22464679914735E-16,0.));
#7678=DIRECTION('center_axis',(0.,0.,-1.));
#7679=DIRECTION('ref_axis',(1.,0.,0.));
#7680=DIRECTION('axis',(0.,0.,1.));
#7681=DIRECTION('refdir',(1.,0.,0.));
#7682=DIRECTION('center_axis',(0.,0.,1.));
#7683=DIRECTION('ref_axis',(1.,0.,0.));
#7684=DIRECTION('center_axis',(0.,0.,1.));
#7685=DIRECTION('ref_axis',(1.,0.,0.));
#7686=DIRECTION('',(0.,0.,1.));
#7687=DIRECTION('center_axis',(0.,0.,1.));
#7688=DIRECTION('ref_axis',(1.,0.,0.));
#7689=DIRECTION('center_axis',(0.,0.,1.));
#7690=DIRECTION('ref_axis',(1.,0.,0.));
#7691=DIRECTION('center_axis',(0.,0.,-1.));
#7692=DIRECTION('ref_axis',(1.,0.,0.));
#7693=DIRECTION('center_axis',(0.,0.,1.));
#7694=DIRECTION('ref_axis',(1.,0.,0.));
#7695=DIRECTION('center_axis',(0.,0.,-1.));
#7696=DIRECTION('ref_axis',(1.,0.,0.));
#7697=DIRECTION('',(0.,0.,-1.));
#7698=DIRECTION('center_axis',(0.,0.,1.));
#7699=DIRECTION('ref_axis',(1.,0.,0.));
#7700=DIRECTION('center_axis',(0.,0.,1.));
#7701=DIRECTION('ref_axis',(1.,0.,0.));
#7702=DIRECTION('',(0.,0.,-1.));
#7703=DIRECTION('center_axis',(0.,0.,1.));
#7704=DIRECTION('ref_axis',(1.,0.,0.));
#7705=DIRECTION('center_axis',(0.,0.,1.));
#7706=DIRECTION('ref_axis',(1.,0.,0.));
#7707=DIRECTION('center_axis',(0.,0.,1.));
#7708=DIRECTION('ref_axis',(1.,0.,0.));
#7709=DIRECTION('axis',(0.,0.,1.));
#7710=DIRECTION('refdir',(1.,0.,0.));
#7711=DIRECTION('center_axis',(0.,0.,1.));
#7712=DIRECTION('ref_axis',(1.,0.,0.));
#7713=DIRECTION('center_axis',(0.,0.,1.));
#7714=DIRECTION('ref_axis',(1.,0.,0.));
#7715=DIRECTION('',(0.,0.,1.));
#7716=DIRECTION('center_axis',(0.,0.,-1.));
#7717=DIRECTION('ref_axis',(1.,0.,0.));
#7718=DIRECTION('center_axis',(0.,0.,1.));
#7719=DIRECTION('ref_axis',(1.,0.,0.));
#7720=DIRECTION('center_axis',(0.,0.,1.));
#7721=DIRECTION('ref_axis',(1.,0.,0.));
#7722=DIRECTION('center_axis',(0.,0.,1.));
#7723=DIRECTION('ref_axis',(1.,0.,0.));
#7724=DIRECTION('',(0.,0.,1.));
#7725=DIRECTION('center_axis',(0.,0.,-1.));
#7726=DIRECTION('ref_axis',(1.,0.,0.));
#7727=DIRECTION('center_axis',(0.,0.,1.));
#7728=DIRECTION('ref_axis',(1.,0.,0.));
#7729=DIRECTION('center_axis',(0.,0.,1.));
#7730=DIRECTION('ref_axis',(1.,0.,0.));
#7731=DIRECTION('center_axis',(0.,0.,1.));
#7732=DIRECTION('ref_axis',(1.,0.,0.));
#7733=DIRECTION('',(0.,0.,1.));
#7734=DIRECTION('center_axis',(0.,0.,-1.));
#7735=DIRECTION('ref_axis',(1.,0.,0.));
#7736=DIRECTION('center_axis',(0.,0.,1.));
#7737=DIRECTION('ref_axis',(1.,0.,0.));
#7738=DIRECTION('center_axis',(0.,0.,1.));
#7739=DIRECTION('ref_axis',(1.,0.,0.));
#7740=DIRECTION('',(0.,0.,1.));
#7741=DIRECTION('center_axis',(0.,0.,-1.));
#7742=DIRECTION('ref_axis',(1.,0.,0.));
#7743=DIRECTION('center_axis',(0.,0.,1.));
#7744=DIRECTION('ref_axis',(1.,0.,0.));
#7745=DIRECTION('center_axis',(0.,0.,1.));
#7746=DIRECTION('ref_axis',(1.,0.,0.));
#7747=DIRECTION('',(0.,0.,1.));
#7748=DIRECTION('center_axis',(0.,0.,-1.));
#7749=DIRECTION('ref_axis',(1.,0.,0.));
#7750=DIRECTION('center_axis',(0.,0.,1.));
#7751=DIRECTION('ref_axis',(1.,0.,0.));
#7752=DIRECTION('center_axis',(0.,0.,1.));
#7753=DIRECTION('ref_axis',(1.,0.,0.));
#7754=DIRECTION('',(0.,0.,1.));
#7755=DIRECTION('center_axis',(0.,0.,-1.));
#7756=DIRECTION('ref_axis',(1.,0.,0.));
#7757=DIRECTION('center_axis',(0.,0.,1.));
#7758=DIRECTION('ref_axis',(1.,0.,0.));
#7759=DIRECTION('center_axis',(0.,0.,1.));
#7760=DIRECTION('ref_axis',(1.,0.,0.));
#7761=DIRECTION('',(0.,0.,1.));
#7762=DIRECTION('center_axis',(0.,0.,-1.));
#7763=DIRECTION('ref_axis',(1.,0.,0.));
#7764=DIRECTION('center_axis',(0.,1.,0.));
#7765=DIRECTION('ref_axis',(-1.,0.,0.));
#7766=DIRECTION('',(-1.,0.,0.));
#7767=DIRECTION('',(0.,0.,1.));
#7768=DIRECTION('',(-1.,0.,0.));
#7769=DIRECTION('',(0.,0.,1.));
#7770=DIRECTION('center_axis',(1.,0.,0.));
#7771=DIRECTION('ref_axis',(0.,1.,0.));
#7772=DIRECTION('',(0.,1.,0.));
#7773=DIRECTION('',(0.,1.,0.));
#7774=DIRECTION('',(0.,0.,1.));
#7775=DIRECTION('center_axis',(0.,-1.,0.));
#7776=DIRECTION('ref_axis',(1.,0.,0.));
#7777=DIRECTION('',(1.,0.,0.));
#7778=DIRECTION('',(1.,0.,0.));
#7779=DIRECTION('',(0.,0.,1.));
#7780=DIRECTION('center_axis',(-1.,0.,0.));
#7781=DIRECTION('ref_axis',(0.,-1.,0.));
#7782=DIRECTION('',(0.,-1.,0.));
#7783=DIRECTION('',(0.,-1.,0.));
#7784=DIRECTION('center_axis',(0.,0.,1.));
#7785=DIRECTION('ref_axis',(1.,0.,0.));
#7786=DIRECTION('center_axis',(0.,0.,1.));
#7787=DIRECTION('ref_axis',(1.,0.,0.));
#7788=DIRECTION('axis',(0.,0.,1.));
#7789=DIRECTION('refdir',(1.,0.,0.));
#7790=DIRECTION('center_axis',(6.12323399573677E-17,0.,1.));
#7791=DIRECTION('ref_axis',(1.,0.,0.));
#7792=DIRECTION('center_axis',(0.,-1.,0.));
#7793=DIRECTION('ref_axis',(0.,0.,-1.));
#7794=DIRECTION('center_axis',(0.,1.,0.));
#7795=DIRECTION('ref_axis',(1.,0.,0.));
#7796=DIRECTION('center_axis',(0.,1.,0.));
#7797=DIRECTION('ref_axis',(1.,0.,0.));
#7798=DIRECTION('',(0.,-1.,0.));
#7799=DIRECTION('center_axis',(0.,-1.,0.));
#7800=DIRECTION('ref_axis',(1.,0.,0.));
#7801=DIRECTION('center_axis',(0.,1.,0.));
#7802=DIRECTION('ref_axis',(1.,0.,0.));
#7803=DIRECTION('center_axis',(0.,1.,0.));
#7804=DIRECTION('ref_axis',(1.,0.,0.));
#7805=DIRECTION('',(0.,-1.,0.));
#7806=DIRECTION('center_axis',(0.,1.,0.));
#7807=DIRECTION('ref_axis',(1.,0.,0.));
#7808=DIRECTION('center_axis',(0.,1.,0.));
#7809=DIRECTION('ref_axis',(1.,0.,0.));
#7810=DIRECTION('center_axis',(0.,1.,0.));
#7811=DIRECTION('ref_axis',(1.,0.,0.));
#7812=DIRECTION('axis',(0.,0.,1.));
#7813=DIRECTION('refdir',(1.,0.,0.));
#7814=DIRECTION('center_axis',(0.866025403784439,0.,-0.5));
#7815=DIRECTION('ref_axis',(0.5,0.,0.866025403784439));
#7816=DIRECTION('',(-0.5,0.,-0.866025403784439));
#7817=DIRECTION('',(0.,-1.,0.));
#7818=DIRECTION('',(0.5,0.,0.866025403784439));
#7819=DIRECTION('',(0.,-1.,0.));
#7820=DIRECTION('center_axis',(1.20185167898973E-16,0.,-1.));
#7821=DIRECTION('ref_axis',(1.,0.,1.20185167898973E-16));
#7822=DIRECTION('',(-1.,0.,-1.20185167898973E-16));
#7823=DIRECTION('',(0.,-1.,0.));
#7824=DIRECTION('',(1.,0.,1.20185167898973E-16));
#7825=DIRECTION('center_axis',(-0.866025403784439,0.,-0.5));
#7826=DIRECTION('ref_axis',(0.5,0.,-0.866025403784439));
#7827=DIRECTION('',(-0.5,0.,0.866025403784439));
#7828=DIRECTION('',(0.,-1.,0.));
#7829=DIRECTION('',(0.5,0.,-0.866025403784439));
#7830=DIRECTION('center_axis',(-0.866025403784439,0.,0.5));
#7831=DIRECTION('ref_axis',(-0.5,0.,-0.866025403784439));
#7832=DIRECTION('',(0.5,0.,0.866025403784439));
#7833=DIRECTION('',(0.,-1.,0.));
#7834=DIRECTION('',(-0.5,0.,-0.866025403784439));
#7835=DIRECTION('center_axis',(-2.40370335797945E-16,0.,1.));
#7836=DIRECTION('ref_axis',(-1.,0.,-2.40370335797945E-16));
#7837=DIRECTION('',(1.,0.,2.40370335797945E-16));
#7838=DIRECTION('',(0.,-1.,0.));
#7839=DIRECTION('',(-1.,0.,-2.40370335797945E-16));
#7840=DIRECTION('center_axis',(0.866025403784439,0.,0.5));
#7841=DIRECTION('ref_axis',(-0.5,0.,0.866025403784439));
#7842=DIRECTION('',(0.5,0.,-0.866025403784439));
#7843=DIRECTION('',(-0.5,0.,0.866025403784439));
#7844=DIRECTION('center_axis',(0.,1.,0.));
#7845=DIRECTION('ref_axis',(1.,0.,0.));
#7846=DIRECTION('center_axis',(0.,-1.,0.));
#7847=DIRECTION('ref_axis',(0.,0.,-1.));
#7848=DIRECTION('center_axis',(0.,1.,0.));
#7849=DIRECTION('ref_axis',(1.,0.,0.));
#7850=DIRECTION('center_axis',(0.,1.,0.));
#7851=DIRECTION('ref_axis',(1.,0.,0.));
#7852=DIRECTION('center_axis',(0.,1.,0.));
#7853=DIRECTION('ref_axis',(1.,0.,0.));
#7854=DIRECTION('center_axis',(0.,1.,0.));
#7855=DIRECTION('ref_axis',(1.,0.,0.));
#7856=DIRECTION('',(0.,-1.,0.));
#7857=DIRECTION('center_axis',(0.,1.,0.));
#7858=DIRECTION('ref_axis',(1.,0.,0.));
#7859=DIRECTION('center_axis',(0.,1.,0.));
#7860=DIRECTION('ref_axis',(1.,0.,0.));
#7861=DIRECTION('center_axis',(0.,1.,0.));
#7862=DIRECTION('ref_axis',(0.,0.,1.));
#7863=DIRECTION('center_axis',(0.,-1.,0.));
#7864=DIRECTION('ref_axis',(1.,0.,0.));
#7865=DIRECTION('center_axis',(0.,-1.,0.));
#7866=DIRECTION('ref_axis',(1.,0.,0.));
#7867=DIRECTION('center_axis',(0.,-1.,0.));
#7868=DIRECTION('ref_axis',(1.,0.,0.));
#7869=DIRECTION('',(0.707106781186548,0.707106781186547,8.65956056235493E-17));
#7870=DIRECTION('center_axis',(0.,-1.,0.));
#7871=DIRECTION('ref_axis',(1.,0.,0.));
#7872=DIRECTION('center_axis',(0.,-1.,0.));
#7873=DIRECTION('ref_axis',(1.,0.,0.));
#7874=DIRECTION('',(0.,1.,0.));
#7875=DIRECTION('center_axis',(0.,1.,0.));
#7876=DIRECTION('ref_axis',(1.,0.,0.));
#7877=DIRECTION('center_axis',(0.,-1.,0.));
#7878=DIRECTION('ref_axis',(1.,0.,0.));
#7879=DIRECTION('',(-0.707106781186547,0.707106781186548,-8.65956056235493E-17));
#7880=DIRECTION('center_axis',(0.,-1.,0.));
#7881=DIRECTION('ref_axis',(0.,0.,-1.));
#7882=DIRECTION('center_axis',(0.,-1.,0.));
#7883=DIRECTION('ref_axis',(1.,0.,0.));
#7884=DIRECTION('center_axis',(0.,1.,0.));
#7885=DIRECTION('ref_axis',(1.,0.,0.));
#7886=DIRECTION('center_axis',(0.,1.,0.));
#7887=DIRECTION('ref_axis',(1.,0.,0.));
#7888=DIRECTION('',(-0.447213595499958,0.894427190999916,-5.47678698264203E-17));
#7889=DIRECTION('center_axis',(0.,-1.,0.));
#7890=DIRECTION('ref_axis',(1.,0.,0.));
#7891=DIRECTION('',(0.,1.,0.));
#7892=DIRECTION('axis',(0.,0.,1.));
#7893=DIRECTION('refdir',(1.,0.,0.));
#7894=DIRECTION('center_axis',(0.,1.,0.));
#7895=DIRECTION('ref_axis',(1.,0.,0.));
#7896=DIRECTION('center_axis',(0.,1.,0.));
#7897=DIRECTION('ref_axis',(1.,0.,0.));
#7898=DIRECTION('',(0.707106781186548,-0.707106781186547,-8.65956056235494E-17));
#7899=DIRECTION('center_axis',(0.,-1.,0.));
#7900=DIRECTION('ref_axis',(1.,0.,0.));
#7901=DIRECTION('center_axis',(0.,1.,0.));
#7902=DIRECTION('ref_axis',(1.,0.,0.));
#7903=DIRECTION('',(0.,-1.,0.));
#7904=DIRECTION('center_axis',(0.,-1.,0.));
#7905=DIRECTION('ref_axis',(1.,0.,0.));
#7906=DIRECTION('center_axis',(0.,1.,0.));
#7907=DIRECTION('ref_axis',(1.,0.,0.));
#7908=DIRECTION('center_axis',(0.,1.,0.));
#7909=DIRECTION('ref_axis',(1.,0.,0.));
#7910=DIRECTION('center_axis',(0.,1.,0.));
#7911=DIRECTION('ref_axis',(1.,0.,0.));
#7912=DIRECTION('',(0.,-1.,0.));
#7913=DIRECTION('center_axis',(0.,1.,0.));
#7914=DIRECTION('ref_axis',(1.,0.,0.));
#7915=DIRECTION('center_axis',(0.,1.,0.));
#7916=DIRECTION('ref_axis',(1.,0.,0.));
#7917=DIRECTION('axis',(0.,0.,1.));
#7918=DIRECTION('refdir',(1.,0.,0.));
#7919=DIRECTION('center_axis',(0.,1.,0.));
#7920=DIRECTION('ref_axis',(1.,0.,0.));
#7921=DIRECTION('',(0.866025403784439,-0.5,1.06057523872491E-16));
#7922=DIRECTION('center_axis',(0.,-1.,0.));
#7923=DIRECTION('ref_axis',(1.,0.,0.));
#7924=DIRECTION('center_axis',(0.,-1.,0.));
#7925=DIRECTION('ref_axis',(1.,0.,0.));
#7926=DIRECTION('center_axis',(0.,1.,0.));
#7927=DIRECTION('ref_axis',(1.,0.,0.));
#7928=DIRECTION('',(-0.866025403784439,-0.5,-1.06057523872491E-16));
#7929=DIRECTION('center_axis',(1.20185167898973E-16,0.,-1.));
#7930=DIRECTION('ref_axis',(-1.,0.,-1.20185167898973E-16));
#7931=DIRECTION('',(0.,1.,0.));
#7932=DIRECTION('',(0.,1.,0.));
#7933=DIRECTION('center_axis',(-0.866025403784439,0.,-0.5));
#7934=DIRECTION('ref_axis',(-0.5,0.,0.866025403784439));
#7935=DIRECTION('',(0.,1.,0.));
#7936=DIRECTION('center_axis',(-0.866025403784439,0.,0.5));
#7937=DIRECTION('ref_axis',(0.5,0.,0.866025403784439));
#7938=DIRECTION('',(0.,1.,0.));
#7939=DIRECTION('center_axis',(0.,1.,0.));
#7940=DIRECTION('ref_axis',(1.,0.,0.));
#7941=DIRECTION('center_axis',(0.,1.,0.));
#7942=DIRECTION('ref_axis',(1.,0.,0.));
#7943=DIRECTION('',(0.,-1.,0.));
#7944=DIRECTION('center_axis',(0.,1.,0.));
#7945=DIRECTION('ref_axis',(1.,0.,0.));
#7946=DIRECTION('center_axis',(-2.40370335797945E-16,0.,1.));
#7947=DIRECTION('ref_axis',(1.,0.,2.40370335797945E-16));
#7948=DIRECTION('',(0.,1.,0.));
#7949=DIRECTION('center_axis',(0.866025403784439,0.,-0.5));
#7950=DIRECTION('ref_axis',(-0.5,0.,-0.866025403784439));
#7951=DIRECTION('',(0.,1.,0.));
#7952=DIRECTION('center_axis',(0.866025403784439,0.,0.5));
#7953=DIRECTION('ref_axis',(0.5,0.,-0.866025403784439));
#7954=DIRECTION('center_axis',(0.,1.,0.));
#7955=DIRECTION('ref_axis',(1.,0.,0.));
#7956=DIRECTION('center_axis',(0.,1.,0.));
#7957=DIRECTION('ref_axis',(1.,0.,0.));
#7958=DIRECTION('axis',(0.,0.,1.));
#7959=DIRECTION('refdir',(1.,0.,0.));
#7960=DIRECTION('center_axis',(0.,1.,0.));
#7961=DIRECTION('ref_axis',(1.,0.,0.));
#7962=DIRECTION('',(-0.5,0.,0.866025403784439));
#7963=DIRECTION('',(-1.,0.,-2.84883360945713E-16));
#7964=DIRECTION('',(-0.5,0.,-0.866025403784439));
#7965=DIRECTION('',(0.5,0.,-0.866025403784439));
#7966=DIRECTION('',(1.,0.,0.));
#7967=DIRECTION('',(0.5,0.,0.866025403784439));
#7968=DIRECTION('center_axis',(0.,-1.,0.));
#7969=DIRECTION('ref_axis',(1.,0.,0.));
#7970=DIRECTION('center_axis',(0.,1.,0.));
#7971=DIRECTION('ref_axis',(1.,0.,0.));
#7972=DIRECTION('',(0.5,0.,-0.866025403784439));
#7973=DIRECTION('',(-0.5,0.,-0.866025403784439));
#7974=DIRECTION('',(-1.,0.,0.));
#7975=DIRECTION('',(-0.5,0.,0.866025403784439));
#7976=DIRECTION('',(0.5,0.,0.866025403784439));
#7977=DIRECTION('',(1.,0.,2.84883360945713E-16));
#7978=DIRECTION('center_axis',(0.,1.,0.));
#7979=DIRECTION('ref_axis',(1.,0.,0.));
#7980=DIRECTION('center_axis',(-2.84883360945713E-16,0.,1.));
#7981=DIRECTION('ref_axis',(1.,0.,2.84883360945713E-16));
#7982=DIRECTION('',(0.,-1.,0.));
#7983=DIRECTION('',(0.,1.,0.));
#7984=DIRECTION('center_axis',(-0.866025403784439,0.,0.5));
#7985=DIRECTION('ref_axis',(0.5,0.,0.866025403784439));
#7986=DIRECTION('',(0.,1.,0.));
#7987=DIRECTION('center_axis',(-0.866025403784439,0.,-0.5));
#7988=DIRECTION('ref_axis',(-0.5,0.,0.866025403784439));
#7989=DIRECTION('',(0.,1.,0.));
#7990=DIRECTION('center_axis',(0.,0.,-1.));
#7991=DIRECTION('ref_axis',(-1.,0.,0.));
#7992=DIRECTION('',(0.,1.,0.));
#7993=DIRECTION('center_axis',(0.866025403784439,0.,-0.5));
#7994=DIRECTION('ref_axis',(-0.5,0.,-0.866025403784439));
#7995=DIRECTION('',(0.,1.,0.));
#7996=DIRECTION('center_axis',(0.866025403784439,0.,0.5));
#7997=DIRECTION('ref_axis',(0.5,0.,-0.866025403784439));
#7998=DIRECTION('center_axis',(0.,-1.,0.));
#7999=DIRECTION('ref_axis',(1.,0.,0.));
#8000=DIRECTION('',(0.,1.,0.));
#8001=DIRECTION('center_axis',(0.,-1.,0.));
#8002=DIRECTION('ref_axis',(1.,0.,0.));
#8003=DIRECTION('center_axis',(0.,1.,0.));
#8004=DIRECTION('ref_axis',(0.,0.,1.));
#8005=DIRECTION('center_axis',(0.,-1.,0.));
#8006=DIRECTION('ref_axis',(1.,0.,0.));
#8007=DIRECTION('center_axis',(0.,-1.,0.));
#8008=DIRECTION('ref_axis',(1.,0.,0.));
#8009=DIRECTION('center_axis',(0.,-1.,0.));
#8010=DIRECTION('ref_axis',(1.,0.,0.));
#8011=DIRECTION('',(0.707106781186547,0.707106781186548,8.65956056235493E-17));
#8012=DIRECTION('center_axis',(0.,-1.,0.));
#8013=DIRECTION('ref_axis',(1.,0.,0.));
#8014=DIRECTION('center_axis',(0.,-1.,0.));
#8015=DIRECTION('ref_axis',(1.,0.,0.));
#8016=DIRECTION('',(0.,1.,0.));
#8017=DIRECTION('center_axis',(0.,1.,0.));
#8018=DIRECTION('ref_axis',(1.,0.,0.));
#8019=DIRECTION('center_axis',(0.,-1.,0.));
#8020=DIRECTION('ref_axis',(1.,0.,0.));
#8021=DIRECTION('',(-0.707106781186547,0.707106781186548,-8.65956056235493E-17));
#8022=DIRECTION('center_axis',(0.,-1.,0.));
#8023=DIRECTION('ref_axis',(0.,0.,-1.));
#8024=DIRECTION('center_axis',(0.,-1.,0.));
#8025=DIRECTION('ref_axis',(1.,0.,0.));
#8026=DIRECTION('center_axis',(0.,-1.,0.));
#8027=DIRECTION('ref_axis',(1.,0.,0.));
#8028=DIRECTION('',(0.,1.,0.));
#8029=DIRECTION('axis',(0.,0.,1.));
#8030=DIRECTION('refdir',(1.,0.,0.));
#8031=DIRECTION('center_axis',(0.,0.,1.));
#8032=DIRECTION('ref_axis',(1.,0.,0.));
#8033=DIRECTION('center_axis',(0.,0.,-1.));
#8034=DIRECTION('ref_axis',(1.,0.,0.));
#8035=DIRECTION('',(0.,0.,-1.));
#8036=DIRECTION('center_axis',(0.,0.,-1.));
#8037=DIRECTION('ref_axis',(1.,0.,0.));
#8038=DIRECTION('center_axis',(0.,0.,1.));
#8039=DIRECTION('ref_axis',(1.,0.,0.));
#8040=DIRECTION('center_axis',(0.,0.,1.));
#8041=DIRECTION('ref_axis',(1.,0.,0.));
#8042=DIRECTION('',(0.,0.,-1.));
#8043=DIRECTION('center_axis',(0.,0.,1.));
#8044=DIRECTION('ref_axis',(1.,0.,0.));
#8045=DIRECTION('center_axis',(0.,0.,1.));
#8046=DIRECTION('ref_axis',(1.,0.,0.));
#8047=DIRECTION('center_axis',(0.,0.,1.));
#8048=DIRECTION('ref_axis',(1.,0.,0.));
#8049=DIRECTION('axis',(0.,0.,1.));
#8050=DIRECTION('refdir',(1.,0.,0.));
#8051=DIRECTION('center_axis',(0.,1.,0.));
#8052=DIRECTION('ref_axis',(0.,0.,1.));
#8053=DIRECTION('center_axis',(0.,-1.,0.));
#8054=DIRECTION('ref_axis',(1.,0.,0.));
#8055=DIRECTION('center_axis',(0.,-1.,0.));
#8056=DIRECTION('ref_axis',(1.,0.,0.));
#8057=DIRECTION('center_axis',(0.,-1.,0.));
#8058=DIRECTION('ref_axis',(1.,0.,0.));
#8059=DIRECTION('',(0.707106781186547,0.707106781186548,8.65956056235493E-17));
#8060=DIRECTION('center_axis',(0.,-1.,0.));
#8061=DIRECTION('ref_axis',(1.,0.,0.));
#8062=DIRECTION('center_axis',(0.,-1.,0.));
#8063=DIRECTION('ref_axis',(1.,0.,0.));
#8064=DIRECTION('',(0.,1.,0.));
#8065=DIRECTION('center_axis',(0.,1.,0.));
#8066=DIRECTION('ref_axis',(1.,0.,0.));
#8067=DIRECTION('center_axis',(0.,-1.,0.));
#8068=DIRECTION('ref_axis',(1.,0.,0.));
#8069=DIRECTION('',(-0.707106781186547,0.707106781186548,-8.65956056235493E-17));
#8070=DIRECTION('center_axis',(0.,-1.,0.));
#8071=DIRECTION('ref_axis',(0.,0.,-1.));
#8072=DIRECTION('center_axis',(0.,-1.,0.));
#8073=DIRECTION('ref_axis',(1.,0.,0.));
#8074=DIRECTION('center_axis',(0.,1.,0.));
#8075=DIRECTION('ref_axis',(1.,0.,0.));
#8076=DIRECTION('center_axis',(0.,1.,0.));
#8077=DIRECTION('ref_axis',(1.,0.,0.));
#8078=DIRECTION('',(-0.447213595499958,0.894427190999916,-5.47678698264203E-17));
#8079=DIRECTION('center_axis',(0.,-1.,0.));
#8080=DIRECTION('ref_axis',(1.,0.,0.));
#8081=DIRECTION('center_axis',(0.,1.,0.));
#8082=DIRECTION('ref_axis',(1.,0.,0.));
#8083=DIRECTION('',(0.,1.,0.));
#8084=DIRECTION('center_axis',(0.,1.,0.));
#8085=DIRECTION('ref_axis',(1.,0.,0.));
#8086=DIRECTION('center_axis',(0.,-1.,0.));
#8087=DIRECTION('ref_axis',(1.,0.,0.));
#8088=DIRECTION('',(-0.707106781186547,0.707106781186548,-8.65956056235493E-17));
#8089=DIRECTION('center_axis',(0.,-1.,0.));
#8090=DIRECTION('ref_axis',(0.,0.,-1.));
#8091=DIRECTION('center_axis',(0.866025403784439,0.,-0.5));
#8092=DIRECTION('ref_axis',(0.5,0.,0.866025403784439));
#8093=DIRECTION('',(-0.5,0.,-0.866025403784439));
#8094=DIRECTION('',(0.,-1.,0.));
#8095=DIRECTION('',(0.5,0.,0.866025403784439));
#8096=DIRECTION('',(0.,-1.,0.));
#8097=DIRECTION('center_axis',(1.60246890531964E-16,0.,-1.));
#8098=DIRECTION('ref_axis',(1.,0.,1.60246890531964E-16));
#8099=DIRECTION('',(-1.,0.,-1.60246890531964E-16));
#8100=DIRECTION('',(0.,-1.,0.));
#8101=DIRECTION('',(1.,0.,1.60246890531964E-16));
#8102=DIRECTION('center_axis',(-0.866025403784439,0.,-0.5));
#8103=DIRECTION('ref_axis',(0.5,0.,-0.866025403784439));
#8104=DIRECTION('',(-0.5,0.,0.866025403784439));
#8105=DIRECTION('',(0.,-1.,0.));
#8106=DIRECTION('',(0.5,0.,-0.866025403784439));
#8107=DIRECTION('center_axis',(-0.866025403784439,0.,0.5));
#8108=DIRECTION('ref_axis',(-0.5,0.,-0.866025403784439));
#8109=DIRECTION('',(0.5,0.,0.866025403784439));
#8110=DIRECTION('',(0.,-1.,0.));
#8111=DIRECTION('',(-0.5,0.,-0.866025403784439));
#8112=DIRECTION('center_axis',(-1.60246890531964E-16,0.,1.));
#8113=DIRECTION('ref_axis',(-1.,0.,-1.60246890531964E-16));
#8114=DIRECTION('',(1.,0.,1.60246890531964E-16));
#8115=DIRECTION('',(0.,-1.,0.));
#8116=DIRECTION('',(-1.,0.,-1.60246890531964E-16));
#8117=DIRECTION('center_axis',(0.866025403784439,0.,0.5));
#8118=DIRECTION('ref_axis',(-0.5,0.,0.866025403784439));
#8119=DIRECTION('',(0.5,0.,-0.866025403784439));
#8120=DIRECTION('',(-0.5,0.,0.866025403784439));
#8121=DIRECTION('center_axis',(0.,1.,0.));
#8122=DIRECTION('ref_axis',(1.,0.,0.));
#8123=DIRECTION('center_axis',(0.,-1.,0.));
#8124=DIRECTION('ref_axis',(0.,0.,-1.));
#8125=DIRECTION('axis',(0.,0.,1.));
#8126=DIRECTION('refdir',(1.,0.,0.));
#8127=DIRECTION('center_axis',(0.,0.,1.));
#8128=DIRECTION('ref_axis',(1.,0.,0.));
#8129=DIRECTION('center_axis',(0.,0.,1.));
#8130=DIRECTION('ref_axis',(1.,0.,0.));
#8131=DIRECTION('',(0.,0.,-1.));
#8132=DIRECTION('center_axis',(0.,0.,1.));
#8133=DIRECTION('ref_axis',(1.,0.,0.));
#8134=DIRECTION('center_axis',(0.,0.,1.));
#8135=DIRECTION('ref_axis',(1.,0.,0.));
#8136=DIRECTION('center_axis',(0.,0.,1.));
#8137=DIRECTION('ref_axis',(1.,0.,0.));
#8138=DIRECTION('axis',(0.,0.,1.));
#8139=DIRECTION('refdir',(1.,0.,0.));
#8140=DIRECTION('center_axis',(0.,1.,0.));
#8141=DIRECTION('ref_axis',(1.,0.,0.));
#8142=DIRECTION('center_axis',(-0.707106781186548,0.707106781186548,0.));
#8143=DIRECTION('ref_axis',(0.707106781186548,0.707106781186548,0.));
#8144=DIRECTION('center_axis',(0.,1.,0.));
#8145=DIRECTION('ref_axis',(1.,-6.03382078600629E-17,0.));
#8146=DIRECTION('',(0.,1.,0.));
#8147=DIRECTION('center_axis',(0.,-1.,0.));
#8148=DIRECTION('ref_axis',(1.,0.,0.));
#8149=DIRECTION('center_axis',(0.,1.,0.));
#8150=DIRECTION('ref_axis',(1.,-6.03382078600629E-17,0.));
#8151=DIRECTION('center_axis',(6.12323399573677E-17,0.,1.));
#8152=DIRECTION('ref_axis',(1.,0.,0.));
#8153=DIRECTION('center_axis',(-1.22464679914735E-16,1.,0.));
#8154=DIRECTION('ref_axis',(-1.,-1.22464679914735E-16,0.));
#8155=DIRECTION('center_axis',(1.,0.,0.));
#8156=DIRECTION('ref_axis',(-6.03382078600629E-17,0.,-1.));
#8157=DIRECTION('center_axis',(1.,0.,0.));
#8158=DIRECTION('ref_axis',(-6.03382078600629E-17,0.,-1.));
#8159=DIRECTION('center_axis',(1.,0.,0.));
#8160=DIRECTION('ref_axis',(0.,0.,-1.));
#8161=DIRECTION('',(1.,0.,0.));
#8162=DIRECTION('center_axis',(-1.,0.,0.));
#8163=DIRECTION('ref_axis',(0.,0.,-1.));
#8164=DIRECTION('center_axis',(0.,-1.,0.));
#8165=DIRECTION('ref_axis',(0.,0.,-1.));
#8166=DIRECTION('center_axis',(0.,-1.,0.));
#8167=DIRECTION('ref_axis',(1.,0.,0.));
#8168=DIRECTION('center_axis',(0.,-1.,0.));
#8169=DIRECTION('ref_axis',(1.,0.,0.));
#8170=DIRECTION('center_axis',(0.,-1.,0.));
#8171=DIRECTION('ref_axis',(1.,0.,0.));
#8172=DIRECTION('',(0.,-1.,0.));
#8173=DIRECTION('center_axis',(1.,0.,0.));
#8174=DIRECTION('ref_axis',(0.,1.,0.));
#8175=DIRECTION('center_axis',(1.,0.,0.));
#8176=DIRECTION('ref_axis',(0.,0.,-1.));
#8177=DIRECTION('',(1.,0.,0.));
#8178=DIRECTION('center_axis',(-1.,0.,0.));
#8179=DIRECTION('ref_axis',(0.,1.,0.));
#8180=DIRECTION('center_axis',(-1.,0.,0.));
#8181=DIRECTION('ref_axis',(0.,0.,1.));
#8182=DIRECTION('center_axis',(6.12323399573677E-17,0.,1.));
#8183=DIRECTION('ref_axis',(1.,0.,0.));
#8184=DIRECTION('center_axis',(0.,-1.,0.));
#8185=DIRECTION('ref_axis',(1.,0.,0.));
#8186=DIRECTION('center_axis',(0.,-1.,0.));
#8187=DIRECTION('ref_axis',(1.,0.,0.));
#8188=DIRECTION('center_axis',(1.,0.,0.));
#8189=DIRECTION('ref_axis',(0.,0.,-1.));
#8190=DIRECTION('center_axis',(1.,0.,0.));
#8191=DIRECTION('ref_axis',(0.,0.,-1.));
#8192=DIRECTION('center_axis',(0.,-1.,0.));
#8193=DIRECTION('ref_axis',(1.,0.,0.));
#8194=DIRECTION('center_axis',(0.707106781186548,-0.707106781186548,0.));
#8195=DIRECTION('ref_axis',(0.707106781186548,0.707106781186547,0.));
#8196=DIRECTION('',(0.,1.,0.));
#8197=DIRECTION('center_axis',(0.,-1.,0.));
#8198=DIRECTION('ref_axis',(1.,0.,0.));
#8199=DIRECTION('center_axis',(0.,1.,0.));
#8200=DIRECTION('ref_axis',(0.,0.,1.));
#8201=DIRECTION('center_axis',(0.,-1.,0.));
#8202=DIRECTION('ref_axis',(1.,0.,0.));
#8203=DIRECTION('center_axis',(0.,-1.,0.));
#8204=DIRECTION('ref_axis',(1.,0.,0.));
#8205=DIRECTION('center_axis',(0.,-1.,0.));
#8206=DIRECTION('ref_axis',(1.,0.,0.));
#8207=DIRECTION('',(0.,1.,0.));
#8208=DIRECTION('center_axis',(0.,-1.,0.));
#8209=DIRECTION('ref_axis',(0.,0.,-1.));
#8210=DIRECTION('center_axis',(-1.,0.,0.));
#8211=DIRECTION('ref_axis',(0.,0.,1.));
#8212=DIRECTION('center_axis',(1.,0.,0.));
#8213=DIRECTION('ref_axis',(0.,0.,-1.));
#8214=DIRECTION('center_axis',(1.,0.,0.));
#8215=DIRECTION('ref_axis',(0.,0.,-1.));
#8216=DIRECTION('center_axis',(1.,0.,0.));
#8217=DIRECTION('ref_axis',(0.,1.,0.));
#8218=DIRECTION('center_axis',(1.,0.,0.));
#8219=DIRECTION('ref_axis',(0.,0.,-1.));
#8220=DIRECTION('',(-1.,0.,0.));
#8221=DIRECTION('center_axis',(1.,0.,0.));
#8222=DIRECTION('ref_axis',(0.,0.,-1.));
#8223=DIRECTION('center_axis',(1.,0.,0.));
#8224=DIRECTION('ref_axis',(0.,1.,0.));
#8225=DIRECTION('',(-1.,0.,0.));
#8226=DIRECTION('axis',(0.,0.,1.));
#8227=DIRECTION('refdir',(1.,0.,0.));
#8228=DIRECTION('center_axis',(0.,1.,0.));
#8229=DIRECTION('ref_axis',(1.,0.,0.));
#8230=DIRECTION('',(-0.5,0.,0.866025403784439));
#8231=DIRECTION('',(-1.,0.,-3.29650746237182E-16));
#8232=DIRECTION('',(-0.5,0.,-0.866025403784439));
#8233=DIRECTION('',(0.5,0.,-0.866025403784438));
#8234=DIRECTION('',(1.,0.,0.));
#8235=DIRECTION('',(0.5,0.,0.866025403784439));
#8236=DIRECTION('center_axis',(0.,-1.,0.));
#8237=DIRECTION('ref_axis',(1.,0.,0.));
#8238=DIRECTION('center_axis',(0.,1.,0.));
#8239=DIRECTION('ref_axis',(1.,0.,0.));
#8240=DIRECTION('',(0.5,0.,-0.866025403784439));
#8241=DIRECTION('',(-0.5,0.,-0.866025403784439));
#8242=DIRECTION('',(-1.,0.,0.));
#8243=DIRECTION('',(-0.5,0.,0.866025403784438));
#8244=DIRECTION('',(0.5,0.,0.866025403784439));
#8245=DIRECTION('',(1.,0.,3.29650746237182E-16));
#8246=DIRECTION('center_axis',(0.,1.,0.));
#8247=DIRECTION('ref_axis',(1.,0.,0.));
#8248=DIRECTION('center_axis',(-3.29650746237182E-16,0.,1.));
#8249=DIRECTION('ref_axis',(1.,0.,3.29650746237182E-16));
#8250=DIRECTION('',(0.,-1.,0.));
#8251=DIRECTION('',(0.,1.,0.));
#8252=DIRECTION('center_axis',(-0.866025403784439,0.,0.5));
#8253=DIRECTION('ref_axis',(0.5,0.,0.866025403784439));
#8254=DIRECTION('',(0.,1.,0.));
#8255=DIRECTION('center_axis',(-0.866025403784439,0.,-0.5));
#8256=DIRECTION('ref_axis',(-0.5,0.,0.866025403784439));
#8257=DIRECTION('',(0.,1.,0.));
#8258=DIRECTION('center_axis',(0.,0.,-1.));
#8259=DIRECTION('ref_axis',(-1.,0.,0.));
#8260=DIRECTION('',(0.,1.,0.));
#8261=DIRECTION('center_axis',(0.866025403784439,0.,-0.5));
#8262=DIRECTION('ref_axis',(-0.5,0.,-0.866025403784439));
#8263=DIRECTION('',(0.,1.,0.));
#8264=DIRECTION('center_axis',(0.866025403784439,0.,0.5));
#8265=DIRECTION('ref_axis',(0.5,0.,-0.866025403784439));
#8266=DIRECTION('center_axis',(0.,-1.,0.));
#8267=DIRECTION('ref_axis',(1.,0.,0.));
#8268=DIRECTION('',(0.,1.,0.));
#8269=DIRECTION('center_axis',(0.,-1.,0.));
#8270=DIRECTION('ref_axis',(1.,0.,0.));
#8271=DIRECTION('center_axis',(0.,1.,0.));
#8272=DIRECTION('ref_axis',(0.,0.,1.));
#8273=DIRECTION('center_axis',(0.,-1.,0.));
#8274=DIRECTION('ref_axis',(1.,0.,0.));
#8275=DIRECTION('center_axis',(0.,-1.,0.));
#8276=DIRECTION('ref_axis',(1.,0.,0.));
#8277=DIRECTION('center_axis',(0.,-1.,0.));
#8278=DIRECTION('ref_axis',(1.,0.,0.));
#8279=DIRECTION('',(0.707106781186547,0.707106781186548,8.65956056235493E-17));
#8280=DIRECTION('center_axis',(0.,-1.,0.));
#8281=DIRECTION('ref_axis',(1.,0.,0.));
#8282=DIRECTION('center_axis',(0.,-1.,0.));
#8283=DIRECTION('ref_axis',(1.,0.,0.));
#8284=DIRECTION('',(0.,1.,0.));
#8285=DIRECTION('center_axis',(0.,1.,0.));
#8286=DIRECTION('ref_axis',(1.,0.,0.));
#8287=DIRECTION('center_axis',(0.,-1.,0.));
#8288=DIRECTION('ref_axis',(1.,0.,0.));
#8289=DIRECTION('',(-0.707106781186547,0.707106781186548,-8.65956056235493E-17));
#8290=DIRECTION('center_axis',(0.,-1.,0.));
#8291=DIRECTION('ref_axis',(0.,0.,-1.));
#8292=DIRECTION('center_axis',(0.,-1.,0.));
#8293=DIRECTION('ref_axis',(1.,0.,0.));
#8294=DIRECTION('center_axis',(0.,-1.,0.));
#8295=DIRECTION('ref_axis',(1.,0.,0.));
#8296=DIRECTION('',(0.,1.,0.));
#8297=DIRECTION('axis',(0.,0.,1.));
#8298=DIRECTION('refdir',(1.,0.,0.));
#8299=DIRECTION('center_axis',(0.,-1.,0.));
#8300=DIRECTION('ref_axis',(1.,0.,0.));
#8301=DIRECTION('center_axis',(0.,1.,0.));
#8302=DIRECTION('ref_axis',(1.,0.,0.));
#8303=DIRECTION('',(0.,1.,0.));
#8304=DIRECTION('center_axis',(0.,-1.,0.));
#8305=DIRECTION('ref_axis',(1.,0.,0.));
#8306=DIRECTION('center_axis',(0.,1.,0.));
#8307=DIRECTION('ref_axis',(1.,0.,0.));
#8308=DIRECTION('center_axis',(0.,-1.,0.));
#8309=DIRECTION('ref_axis',(1.,0.,0.));
#8310=DIRECTION('',(-0.707106781186547,0.707106781186548,-8.65956056235493E-17));
#8311=DIRECTION('center_axis',(0.,-1.,0.));
#8312=DIRECTION('ref_axis',(0.,0.,-1.));
#8313=DIRECTION('center_axis',(0.,-1.,0.));
#8314=DIRECTION('ref_axis',(1.,0.,0.));
#8315=DIRECTION('center_axis',(0.,1.,0.));
#8316=DIRECTION('ref_axis',(1.,0.,0.));
#8317=DIRECTION('',(-0.866025403784439,-0.5,-1.06057523872491E-16));
#8318=DIRECTION('center_axis',(1.92296268638356E-16,0.,-1.));
#8319=DIRECTION('ref_axis',(-1.,0.,-1.92296268638356E-16));
#8320=DIRECTION('',(0.,1.,0.));
#8321=DIRECTION('',(-1.,0.,-1.92296268638356E-16));
#8322=DIRECTION('',(0.,1.,0.));
#8323=DIRECTION('center_axis',(0.866025403784439,0.,-0.5));
#8324=DIRECTION('ref_axis',(-0.5,0.,-0.866025403784439));
#8325=DIRECTION('',(0.,1.,0.));
#8326=DIRECTION('',(-0.5,0.,-0.866025403784439));
#8327=DIRECTION('center_axis',(0.866025403784439,0.,0.5));
#8328=DIRECTION('ref_axis',(0.5,0.,-0.866025403784439));
#8329=DIRECTION('',(0.,1.,0.));
#8330=DIRECTION('',(0.5,0.,-0.866025403784439));
#8331=DIRECTION('center_axis',(-1.92296268638356E-16,0.,1.));
#8332=DIRECTION('ref_axis',(1.,0.,1.92296268638356E-16));
#8333=DIRECTION('',(0.,1.,0.));
#8334=DIRECTION('',(1.,0.,1.92296268638356E-16));
#8335=DIRECTION('center_axis',(-0.866025403784439,0.,0.5));
#8336=DIRECTION('ref_axis',(0.5,0.,0.866025403784439));
#8337=DIRECTION('',(0.,1.,0.));
#8338=DIRECTION('',(0.5,0.,0.866025403784439));
#8339=DIRECTION('center_axis',(-0.866025403784439,0.,-0.5));
#8340=DIRECTION('ref_axis',(-0.5,0.,0.866025403784439));
#8341=DIRECTION('',(-0.5,0.,0.866025403784438));
#8342=DIRECTION('center_axis',(0.,1.,0.));
#8343=DIRECTION('ref_axis',(0.,0.,1.));
#8344=DIRECTION('center_axis',(0.,1.,0.));
#8345=DIRECTION('ref_axis',(1.,0.,0.));
#8346=DIRECTION('',(0.,0.,1.));
#8347=DIRECTION('',(1.,0.,0.));
#8348=DIRECTION('',(0.,0.,1.));
#8349=DIRECTION('',(1.,0.,0.));
#8350=DIRECTION('',(0.,0.,1.));
#8351=DIRECTION('',(1.,0.,0.));
#8352=DIRECTION('',(0.,0.,1.));
#8353=DIRECTION('',(1.,0.,0.));
#8354=DIRECTION('',(0.,0.,1.));
#8355=DIRECTION('',(1.,0.,0.));
#8356=DIRECTION('',(0.,0.,1.));
#8357=DIRECTION('',(1.,0.,0.));
#8358=DIRECTION('',(0.,0.,1.));
#8359=DIRECTION('',(1.,0.,0.));
#8360=DIRECTION('',(0.,0.,1.));
#8361=DIRECTION('',(1.,0.,0.));
#8362=DIRECTION('',(0.,0.,1.));
#8363=DIRECTION('',(1.,0.,0.));
#8364=DIRECTION('',(0.,0.,1.));
#8365=DIRECTION('',(1.,0.,0.));
#8366=DIRECTION('',(0.,0.,1.));
#8367=DIRECTION('',(1.,0.,0.));
#8368=DIRECTION('',(0.,0.,1.));
#8369=DIRECTION('',(1.,0.,0.));
#8370=DIRECTION('',(0.,0.,1.));
#8371=DIRECTION('',(1.,0.,0.));
#8372=DIRECTION('',(0.,0.,1.));
#8373=DIRECTION('',(-1.,1.22464679914735E-16,0.));
#8374=DIRECTION('',(0.,0.,1.));
#8375=DIRECTION('',(-1.,1.22464679914735E-16,0.));
#8376=DIRECTION('',(0.,0.,1.));
#8377=DIRECTION('',(-1.,1.22464679914735E-16,0.));
#8378=DIRECTION('',(0.,0.,1.));
#8379=DIRECTION('',(1.,0.,0.));
#8380=DIRECTION('',(0.,0.,1.));
#8381=DIRECTION('',(1.,0.,0.));
#8382=DIRECTION('',(0.,0.,1.));
#8383=DIRECTION('',(-1.,1.22464679914735E-16,0.));
#8384=DIRECTION('',(0.,0.,1.));
#8385=DIRECTION('',(-1.,1.22464679914735E-16,0.));
#8386=DIRECTION('',(0.,0.,1.));
#8387=DIRECTION('',(1.,0.,0.));
#8388=DIRECTION('',(0.,0.,1.));
#8389=DIRECTION('',(1.,0.,0.));
#8390=DIRECTION('',(0.,0.,1.));
#8391=DIRECTION('',(-1.,1.22464679914735E-16,0.));
#8392=DIRECTION('',(0.,0.,1.));
#8393=DIRECTION('',(-1.,1.22464679914735E-16,0.));
#8394=DIRECTION('',(0.,0.,1.));
#8395=DIRECTION('',(1.,0.,0.));
#8396=DIRECTION('',(0.,0.,1.));
#8397=DIRECTION('',(1.,0.,0.));
#8398=DIRECTION('',(0.,0.,1.));
#8399=DIRECTION('',(-1.,1.22464679914735E-16,0.));
#8400=DIRECTION('',(0.,0.,1.));
#8401=DIRECTION('',(-1.,1.22464679914735E-16,0.));
#8402=DIRECTION('',(0.,0.,1.));
#8403=DIRECTION('',(1.,0.,0.));
#8404=DIRECTION('',(0.,0.,1.));
#8405=DIRECTION('',(1.,0.,0.));
#8406=DIRECTION('',(0.,0.,1.));
#8407=DIRECTION('',(1.,0.,0.));
#8408=DIRECTION('',(0.,0.,1.));
#8409=DIRECTION('',(1.,0.,0.));
#8410=DIRECTION('',(0.,0.,1.));
#8411=DIRECTION('',(1.,0.,0.));
#8412=DIRECTION('',(0.,-1.,2.22044604925031E-16));
#8413=DIRECTION('',(1.,0.,0.));
#8414=DIRECTION('',(0.,0.,1.));
#8415=DIRECTION('',(1.,0.,0.));
#8416=DIRECTION('',(0.,-1.,2.22044604925031E-16));
#8417=DIRECTION('',(1.,0.,0.));
#8418=DIRECTION('',(0.,0.,1.));
#8419=DIRECTION('',(1.,0.,0.));
#8420=DIRECTION('',(0.,-1.,2.22044604925031E-16));
#8421=DIRECTION('',(1.,0.,0.));
#8422=DIRECTION('',(0.,0.,1.));
#8423=DIRECTION('',(1.,0.,0.));
#8424=DIRECTION('',(0.,-1.,2.22044604925031E-16));
#8425=DIRECTION('',(1.,0.,0.));
#8426=DIRECTION('',(0.,0.,1.));
#8427=DIRECTION('',(1.,0.,0.));
#8428=DIRECTION('',(0.,0.,1.));
#8429=DIRECTION('',(1.,0.,0.));
#8430=DIRECTION('',(0.,0.,1.));
#8431=DIRECTION('',(1.,0.,0.));
#8432=DIRECTION('',(1.22464679914735E-16,0.,-1.));
#8433=DIRECTION('',(-1.,0.,-1.22464679914735E-16));
#8434=DIRECTION('',(0.,0.,1.));
#8435=DIRECTION('',(2.22044604925031E-16,-1.,0.));
#8436=DIRECTION('',(0.,-1.,2.22044604925031E-16));
#8437=DIRECTION('',(1.,0.,0.));
#8438=DIRECTION('',(0.,-1.,2.22044604925031E-16));
#8439=DIRECTION('',(1.,0.,0.));
#8440=DIRECTION('axis',(0.,0.,1.));
#8441=DIRECTION('refdir',(1.,0.,0.));
#8442=DIRECTION('axis',(0.,0.,1.));
#8443=DIRECTION('refdir',(1.,0.,0.));
#8444=DIRECTION('center_axis',(0.,-1.,0.));
#8445=DIRECTION('ref_axis',(1.,0.,0.));
#8446=DIRECTION('center_axis',(0.,-1.,0.));
#8447=DIRECTION('ref_axis',(0.,0.,1.));
#8448=DIRECTION('',(0.,0.,1.));
#8449=DIRECTION('',(1.,0.,0.));
#8450=DIRECTION('',(0.,0.,1.));
#8451=DIRECTION('center_axis',(-1.,0.,0.));
#8452=DIRECTION('ref_axis',(0.,-1.,0.));
#8453=DIRECTION('center_axis',(-1.,0.,0.));
#8454=DIRECTION('ref_axis',(0.,0.,-1.));
#8455=DIRECTION('',(0.,-1.,0.));
#8456=DIRECTION('',(0.,0.,1.));
#8457=DIRECTION('center_axis',(-1.,0.,0.));
#8458=DIRECTION('ref_axis',(0.,0.,-1.));
#8459=DIRECTION('center_axis',(0.,1.,0.));
#8460=DIRECTION('ref_axis',(-1.,0.,0.));
#8461=DIRECTION('center_axis',(0.,1.,0.));
#8462=DIRECTION('ref_axis',(0.,0.,-1.));
#8463=DIRECTION('',(-1.,0.,0.));
#8464=DIRECTION('',(0.,0.,1.));
#8465=DIRECTION('center_axis',(1.,0.,0.));
#8466=DIRECTION('ref_axis',(0.,1.,0.));
#8467=DIRECTION('center_axis',(1.,0.,0.));
#8468=DIRECTION('ref_axis',(0.,0.,1.));
#8469=DIRECTION('',(0.,1.,0.));
#8470=DIRECTION('center_axis',(0.,0.,1.));
#8471=DIRECTION('ref_axis',(1.,0.,0.));
#8472=DIRECTION('center_axis',(0.,1.,0.));
#8473=DIRECTION('ref_axis',(1.,0.,0.));
#8474=DIRECTION('center_axis',(0.,1.,0.));
#8475=DIRECTION('ref_axis',(1.,0.,0.));
#8476=DIRECTION('',(0.,1.,0.));
#8477=DIRECTION('center_axis',(0.,-1.,0.));
#8478=DIRECTION('ref_axis',(1.,0.,0.));
#8479=DIRECTION('center_axis',(6.12323399573677E-17,0.,1.));
#8480=DIRECTION('ref_axis',(1.,0.,0.));
#8481=DIRECTION('center_axis',(1.22464679914735E-16,-1.,0.));
#8482=DIRECTION('ref_axis',(-1.,-1.22464679914735E-16,0.));
#8483=DIRECTION('axis',(0.,0.,1.));
#8484=DIRECTION('refdir',(1.,0.,0.));
#8485=DIRECTION('center_axis',(0.,0.,1.));
#8486=DIRECTION('ref_axis',(1.,0.,0.));
#8487=DIRECTION('center_axis',(0.,0.,1.));
#8488=DIRECTION('ref_axis',(1.,0.,0.));
#8489=DIRECTION('',(0.,0.,1.));
#8490=DIRECTION('center_axis',(0.,0.,-1.));
#8491=DIRECTION('ref_axis',(1.,0.,0.));
#8492=DIRECTION('center_axis',(0.,0.,1.));
#8493=DIRECTION('ref_axis',(1.,0.,0.));
#8494=DIRECTION('center_axis',(0.,0.,1.));
#8495=DIRECTION('ref_axis',(1.,0.,0.));
#8496=DIRECTION('center_axis',(0.,0.,1.));
#8497=DIRECTION('ref_axis',(1.,0.,0.));
#8498=DIRECTION('',(0.,-1.,0.));
#8499=DIRECTION('',(-1.,0.,0.));
#8500=DIRECTION('center_axis',(0.,0.,1.));
#8501=DIRECTION('ref_axis',(1.,0.,0.));
#8502=DIRECTION('center_axis',(0.,0.,1.));
#8503=DIRECTION('ref_axis',(1.,0.,0.));
#8504=DIRECTION('',(1.,0.,0.));
#8505=DIRECTION('',(0.,-1.,0.));
#8506=DIRECTION('center_axis',(0.,0.,1.));
#8507=DIRECTION('ref_axis',(1.,0.,0.));
#8508=DIRECTION('center_axis',(0.,0.,1.));
#8509=DIRECTION('ref_axis',(1.,0.,0.));
#8510=DIRECTION('',(0.,1.,0.));
#8511=DIRECTION('',(1.,0.,0.));
#8512=DIRECTION('center_axis',(0.,0.,1.));
#8513=DIRECTION('ref_axis',(1.,0.,0.));
#8514=DIRECTION('center_axis',(0.,0.,1.));
#8515=DIRECTION('ref_axis',(1.,0.,0.));
#8516=DIRECTION('',(-1.,0.,0.));
#8517=DIRECTION('',(0.,1.,0.));
#8518=DIRECTION('center_axis',(0.,1.,0.));
#8519=DIRECTION('ref_axis',(-1.,0.,0.));
#8520=DIRECTION('',(1.,0.,0.));
#8521=DIRECTION('',(0.,0.,1.));
#8522=DIRECTION('',(-1.,0.,0.));
#8523=DIRECTION('',(0.,0.,1.));
#8524=DIRECTION('center_axis',(1.,0.,0.));
#8525=DIRECTION('ref_axis',(0.,1.,0.));
#8526=DIRECTION('',(0.,-1.,0.));
#8527=DIRECTION('',(0.,1.,0.));
#8528=DIRECTION('',(0.,0.,1.));
#8529=DIRECTION('center_axis',(0.,-1.,0.));
#8530=DIRECTION('ref_axis',(1.,0.,0.));
#8531=DIRECTION('',(-1.,0.,0.));
#8532=DIRECTION('',(1.,0.,0.));
#8533=DIRECTION('',(0.,0.,1.));
#8534=DIRECTION('center_axis',(-1.,0.,0.));
#8535=DIRECTION('ref_axis',(0.,-1.,0.));
#8536=DIRECTION('',(0.,1.,0.));
#8537=DIRECTION('',(0.,-1.,0.));
#8538=DIRECTION('center_axis',(0.,0.,1.));
#8539=DIRECTION('ref_axis',(1.,0.,0.));
#8540=DIRECTION('center_axis',(0.,0.,1.));
#8541=DIRECTION('ref_axis',(1.,0.,0.));
#8542=DIRECTION('center_axis',(0.,0.,1.));
#8543=DIRECTION('ref_axis',(1.,0.,0.));
#8544=DIRECTION('center_axis',(0.,0.,1.));
#8545=DIRECTION('ref_axis',(1.,0.,0.));
#8546=DIRECTION('center_axis',(0.,0.,1.));
#8547=DIRECTION('ref_axis',(1.,0.,0.));
#8548=DIRECTION('center_axis',(0.,0.,1.));
#8549=DIRECTION('ref_axis',(1.,0.,0.));
#8550=DIRECTION('center_axis',(0.,0.,1.));
#8551=DIRECTION('ref_axis',(1.,0.,0.));
#8552=DIRECTION('center_axis',(0.,0.,1.));
#8553=DIRECTION('ref_axis',(1.,0.,0.));
#8554=DIRECTION('center_axis',(0.,0.,1.));
#8555=DIRECTION('ref_axis',(1.,0.,0.));
#8556=DIRECTION('center_axis',(0.,0.,1.));
#8557=DIRECTION('ref_axis',(1.,0.,0.));
#8558=DIRECTION('center_axis',(0.,1.,0.));
#8559=DIRECTION('ref_axis',(-1.,0.,0.));
#8560=DIRECTION('',(-1.,0.,0.));
#8561=DIRECTION('',(0.,0.,1.));
#8562=DIRECTION('',(-1.,0.,0.));
#8563=DIRECTION('',(0.,0.,1.));
#8564=DIRECTION('center_axis',(1.,0.,0.));
#8565=DIRECTION('ref_axis',(0.,1.,0.));
#8566=DIRECTION('',(0.,1.,0.));
#8567=DIRECTION('',(0.,1.,0.));
#8568=DIRECTION('',(0.,0.,1.));
#8569=DIRECTION('center_axis',(0.,-1.,0.));
#8570=DIRECTION('ref_axis',(1.,0.,0.));
#8571=DIRECTION('',(1.,0.,0.));
#8572=DIRECTION('',(1.,0.,0.));
#8573=DIRECTION('',(0.,0.,1.));
#8574=DIRECTION('center_axis',(-1.,0.,0.));
#8575=DIRECTION('ref_axis',(0.,-1.,0.));
#8576=DIRECTION('',(0.,-1.,0.));
#8577=DIRECTION('',(0.,-1.,0.));
#8578=DIRECTION('center_axis',(0.,0.,1.));
#8579=DIRECTION('ref_axis',(1.,0.,0.));
#8580=DIRECTION('center_axis',(0.,0.,1.));
#8581=DIRECTION('ref_axis',(1.,0.,0.));
#8582=DIRECTION('',(0.,0.,-1.));
#8583=DIRECTION('center_axis',(0.,0.,1.));
#8584=DIRECTION('ref_axis',(1.,0.,0.));
#8585=DIRECTION('center_axis',(0.,0.,1.));
#8586=DIRECTION('ref_axis',(1.,0.,0.));
#8587=DIRECTION('axis',(0.,0.,1.));
#8588=DIRECTION('refdir',(1.,0.,0.));
#8589=DIRECTION('center_axis',(0.,-1.,0.));
#8590=DIRECTION('ref_axis',(1.,0.,0.));
#8591=DIRECTION('',(-1.,0.,0.));
#8592=DIRECTION('',(0.,0.,1.));
#8593=DIRECTION('',(1.,0.,0.));
#8594=DIRECTION('',(0.,0.,1.));
#8595=DIRECTION('center_axis',(-1.,0.,0.));
#8596=DIRECTION('ref_axis',(0.,-1.,0.));
#8597=DIRECTION('',(0.,1.,0.));
#8598=DIRECTION('',(0.,-1.,0.));
#8599=DIRECTION('',(0.,0.,1.));
#8600=DIRECTION('center_axis',(0.,1.,0.));
#8601=DIRECTION('ref_axis',(-1.,0.,0.));
#8602=DIRECTION('',(1.,0.,0.));
#8603=DIRECTION('',(-1.,0.,0.));
#8604=DIRECTION('',(0.,0.,1.));
#8605=DIRECTION('center_axis',(1.,0.,0.));
#8606=DIRECTION('ref_axis',(0.,1.,0.));
#8607=DIRECTION('',(0.,-1.,0.));
#8608=DIRECTION('',(0.,1.,0.));
#8609=DIRECTION('center_axis',(0.,1.,0.));
#8610=DIRECTION('ref_axis',(-1.,0.,0.));
#8611=DIRECTION('',(-1.,0.,0.));
#8612=DIRECTION('',(0.,0.,1.));
#8613=DIRECTION('',(-1.,0.,0.));
#8614=DIRECTION('',(0.,0.,1.));
#8615=DIRECTION('center_axis',(1.,0.,0.));
#8616=DIRECTION('ref_axis',(0.,1.,0.));
#8617=DIRECTION('',(0.,1.,0.));
#8618=DIRECTION('',(0.,1.,0.));
#8619=DIRECTION('',(0.,0.,1.));
#8620=DIRECTION('center_axis',(0.,-1.,0.));
#8621=DIRECTION('ref_axis',(1.,0.,0.));
#8622=DIRECTION('',(1.,0.,0.));
#8623=DIRECTION('',(1.,0.,0.));
#8624=DIRECTION('',(0.,0.,1.));
#8625=DIRECTION('center_axis',(-1.,0.,0.));
#8626=DIRECTION('ref_axis',(0.,-1.,0.));
#8627=DIRECTION('',(0.,-1.,0.));
#8628=DIRECTION('',(0.,-1.,0.));
#8629=DIRECTION('center_axis',(0.,0.,1.));
#8630=DIRECTION('ref_axis',(1.,0.,0.));
#8631=DIRECTION('center_axis',(0.,0.,1.));
#8632=DIRECTION('ref_axis',(1.,0.,0.));
#8633=DIRECTION('axis',(0.,0.,1.));
#8634=DIRECTION('refdir',(1.,0.,0.));
#8635=DIRECTION('center_axis',(0.,0.,1.));
#8636=DIRECTION('ref_axis',(1.,0.,0.));
#8637=DIRECTION('center_axis',(0.,0.,-1.));
#8638=DIRECTION('ref_axis',(1.,0.,0.));
#8639=DIRECTION('',(0.,0.,-1.));
#8640=DIRECTION('center_axis',(0.,0.,-1.));
#8641=DIRECTION('ref_axis',(1.,0.,0.));
#8642=DIRECTION('center_axis',(0.,0.,1.));
#8643=DIRECTION('ref_axis',(1.,0.,0.));
#8644=DIRECTION('center_axis',(0.,0.,1.));
#8645=DIRECTION('ref_axis',(1.,0.,0.));
#8646=DIRECTION('',(0.,0.,-1.));
#8647=DIRECTION('center_axis',(0.,0.,1.));
#8648=DIRECTION('ref_axis',(1.,0.,0.));
#8649=DIRECTION('center_axis',(0.,0.,1.));
#8650=DIRECTION('ref_axis',(1.,0.,0.));
#8651=DIRECTION('center_axis',(0.,0.,1.));
#8652=DIRECTION('ref_axis',(1.,0.,0.));
#8653=DIRECTION('axis',(0.,0.,1.));
#8654=DIRECTION('refdir',(1.,0.,0.));
#8655=DIRECTION('center_axis',(0.,1.,0.));
#8656=DIRECTION('ref_axis',(-1.,0.,0.));
#8657=DIRECTION('',(-1.,0.,0.));
#8658=DIRECTION('',(0.,0.,1.));
#8659=DIRECTION('',(-1.,0.,0.));
#8660=DIRECTION('',(0.,0.,1.));
#8661=DIRECTION('center_axis',(1.,0.,0.));
#8662=DIRECTION('ref_axis',(0.,1.,0.));
#8663=DIRECTION('',(0.,1.,0.));
#8664=DIRECTION('',(0.,1.,0.));
#8665=DIRECTION('',(0.,0.,1.));
#8666=DIRECTION('center_axis',(0.,-1.,0.));
#8667=DIRECTION('ref_axis',(1.,0.,0.));
#8668=DIRECTION('',(1.,0.,0.));
#8669=DIRECTION('',(1.,0.,0.));
#8670=DIRECTION('',(0.,0.,1.));
#8671=DIRECTION('center_axis',(-1.,0.,0.));
#8672=DIRECTION('ref_axis',(0.,-1.,0.));
#8673=DIRECTION('',(0.,-1.,0.));
#8674=DIRECTION('',(0.,-1.,0.));
#8675=DIRECTION('center_axis',(0.,0.,1.));
#8676=DIRECTION('ref_axis',(1.,0.,0.));
#8677=DIRECTION('center_axis',(0.,0.,1.));
#8678=DIRECTION('ref_axis',(1.,0.,0.));
#8679=DIRECTION('axis',(0.,0.,1.));
#8680=DIRECTION('refdir',(1.,0.,0.));
#8681=DIRECTION('center_axis',(0.866025403784439,0.,-0.5));
#8682=DIRECTION('ref_axis',(0.5,0.,0.866025403784439));
#8683=DIRECTION('',(-0.5,0.,-0.866025403784439));
#8684=DIRECTION('',(0.,-1.,0.));
#8685=DIRECTION('',(0.5,0.,0.866025403784439));
#8686=DIRECTION('',(0.,-1.,0.));
#8687=DIRECTION('center_axis',(1.60246890531964E-16,0.,-1.));
#8688=DIRECTION('ref_axis',(1.,0.,1.60246890531964E-16));
#8689=DIRECTION('',(-1.,0.,-1.60246890531964E-16));
#8690=DIRECTION('',(0.,-1.,0.));
#8691=DIRECTION('',(1.,0.,1.60246890531964E-16));
#8692=DIRECTION('center_axis',(-0.866025403784439,0.,-0.5));
#8693=DIRECTION('ref_axis',(0.5,0.,-0.866025403784439));
#8694=DIRECTION('',(-0.5,0.,0.866025403784439));
#8695=DIRECTION('',(0.,-1.,0.));
#8696=DIRECTION('',(0.5,0.,-0.866025403784439));
#8697=DIRECTION('center_axis',(-0.866025403784439,0.,0.5));
#8698=DIRECTION('ref_axis',(-0.5,0.,-0.866025403784439));
#8699=DIRECTION('',(0.5,0.,0.866025403784439));
#8700=DIRECTION('',(0.,-1.,0.));
#8701=DIRECTION('',(-0.5,0.,-0.866025403784439));
#8702=DIRECTION('center_axis',(-1.60246890531964E-16,0.,1.));
#8703=DIRECTION('ref_axis',(-1.,0.,-1.60246890531964E-16));
#8704=DIRECTION('',(1.,0.,1.60246890531964E-16));
#8705=DIRECTION('',(0.,-1.,0.));
#8706=DIRECTION('',(-1.,0.,-1.60246890531964E-16));
#8707=DIRECTION('center_axis',(0.866025403784439,0.,0.5));
#8708=DIRECTION('ref_axis',(-0.5,0.,0.866025403784439));
#8709=DIRECTION('',(0.5,0.,-0.866025403784439));
#8710=DIRECTION('',(-0.5,0.,0.866025403784439));
#8711=DIRECTION('center_axis',(0.,1.,0.));
#8712=DIRECTION('ref_axis',(1.,0.,0.));
#8713=DIRECTION('center_axis',(0.,-1.,0.));
#8714=DIRECTION('ref_axis',(0.,0.,-1.));
#8715=DIRECTION('center_axis',(0.,1.,0.));
#8716=DIRECTION('ref_axis',(1.,0.,0.));
#8717=DIRECTION('center_axis',(0.,1.,0.));
#8718=DIRECTION('ref_axis',(1.,0.,0.));
#8719=DIRECTION('center_axis',(0.,1.,0.));
#8720=DIRECTION('ref_axis',(0.,0.,1.));
#8721=DIRECTION('center_axis',(0.,-1.,0.));
#8722=DIRECTION('ref_axis',(1.,0.,0.));
#8723=DIRECTION('center_axis',(0.,-1.,0.));
#8724=DIRECTION('ref_axis',(1.,0.,0.));
#8725=DIRECTION('center_axis',(0.,-1.,0.));
#8726=DIRECTION('ref_axis',(1.,0.,0.));
#8727=DIRECTION('',(0.707106781186547,0.707106781186548,8.65956056235493E-17));
#8728=DIRECTION('center_axis',(0.,-1.,0.));
#8729=DIRECTION('ref_axis',(1.,0.,0.));
#8730=DIRECTION('center_axis',(0.,-1.,0.));
#8731=DIRECTION('ref_axis',(1.,0.,0.));
#8732=DIRECTION('',(0.,1.,0.));
#8733=DIRECTION('center_axis',(0.,1.,0.));
#8734=DIRECTION('ref_axis',(1.,0.,0.));
#8735=DIRECTION('center_axis',(0.,-1.,0.));
#8736=DIRECTION('ref_axis',(1.,0.,0.));
#8737=DIRECTION('',(-0.707106781186547,0.707106781186548,-8.65956056235493E-17));
#8738=DIRECTION('center_axis',(0.,-1.,0.));
#8739=DIRECTION('ref_axis',(0.,0.,-1.));
#8740=DIRECTION('center_axis',(0.,-1.,0.));
#8741=DIRECTION('ref_axis',(1.,0.,0.));
#8742=DIRECTION('center_axis',(0.,1.,0.));
#8743=DIRECTION('ref_axis',(1.,0.,0.));
#8744=DIRECTION('center_axis',(0.,1.,0.));
#8745=DIRECTION('ref_axis',(1.,0.,0.));
#8746=DIRECTION('',(-0.447213595499958,0.894427190999916,-5.47678698264203E-17));
#8747=DIRECTION('center_axis',(0.,-1.,0.));
#8748=DIRECTION('ref_axis',(1.,0.,0.));
#8749=DIRECTION('',(0.,1.,0.));
#8750=DIRECTION('',(0.,0.,1.));
#8751=DIRECTION('',(1.,0.,0.));
#8752=DIRECTION('',(0.,0.,1.));
#8753=DIRECTION('',(1.,0.,0.));
#8754=DIRECTION('',(0.,0.,1.));
#8755=DIRECTION('',(1.,0.,0.));
#8756=DIRECTION('',(0.,0.,1.));
#8757=DIRECTION('',(1.,0.,0.));
#8758=DIRECTION('',(0.,0.,1.));
#8759=DIRECTION('',(1.,0.,0.));
#8760=DIRECTION('',(0.,-1.,2.22044604925031E-16));
#8761=DIRECTION('',(1.,0.,0.));
#8762=DIRECTION('',(0.,0.,1.));
#8763=DIRECTION('',(1.,0.,0.));
#8764=DIRECTION('',(6.12323399573677E-17,5.4768632793512E-34,1.));
#8765=DIRECTION('',(6.45100292628875E-17,-1.,-9.86076094745178E-32));
#8766=CARTESIAN_POINT('',(0.,0.,0.));
#8767=CARTESIAN_POINT('',(0.,0.,0.));
#8768=CARTESIAN_POINT('',(0.,0.,0.));
#8769=CARTESIAN_POINT('Origin',(0.,-8.6,5.));
#8770=CARTESIAN_POINT('',(-0.685,-8.5,5.));
#8771=CARTESIAN_POINT('Origin',(0.,-8.5,5.));
#8772=CARTESIAN_POINT('',(-0.685,-7.3,5.));
#8773=CARTESIAN_POINT('',(-0.685,-8.6,5.));
#8774=CARTESIAN_POINT('Origin',(0.,-7.3,5.));
#8775=CARTESIAN_POINT('Origin',(0.,-7.3,5.));
#8776=CARTESIAN_POINT('',(-0.46,-7.3,5.));
#8777=CARTESIAN_POINT('Origin',(0.,-7.3,5.));
#8778=CARTESIAN_POINT('Origin',(0.,-7.,5.));
#8779=CARTESIAN_POINT('',(-1.065,-7.,5.));
#8780=CARTESIAN_POINT('Origin',(0.,-7.,5.));
#8781=CARTESIAN_POINT('',(-1.065,-5.5,5.));
#8782=CARTESIAN_POINT('',(-1.065,-7.,5.));
#8783=CARTESIAN_POINT('Origin',(0.,-5.5,5.));
#8784=CARTESIAN_POINT('Origin',(0.,-7.,5.));
#8785=CARTESIAN_POINT('',(-0.46,-7.,5.));
#8786=CARTESIAN_POINT('Origin',(0.,-7.,5.));
#8787=CARTESIAN_POINT('Origin',(0.,-8.5,5.));
#8788=CARTESIAN_POINT('',(-0.46,-8.5,5.));
#8789=CARTESIAN_POINT('Origin',(0.,-8.5,5.));
#8790=CARTESIAN_POINT('',(-1.5,-5.5,5.));
#8791=CARTESIAN_POINT('Origin',(0.,-5.5,5.));
#8792=CARTESIAN_POINT('',(-1.5,-8.5,5.));
#8793=CARTESIAN_POINT('',(-1.5,-8.5,5.));
#8794=CARTESIAN_POINT('Origin',(0.,-8.5,5.));
#8795=CARTESIAN_POINT('Origin',(0.,-5.5,5.));
#8796=CARTESIAN_POINT('Origin',(0.,-8.5,5.));
#8797=CARTESIAN_POINT('',(0.,0.,0.));
#8798=CARTESIAN_POINT('Origin',(0.,7.3,5.));
#8799=CARTESIAN_POINT('',(-0.685,7.3,5.));
#8800=CARTESIAN_POINT('Origin',(0.,7.3,5.));
#8801=CARTESIAN_POINT('',(-0.685,8.5,5.));
#8802=CARTESIAN_POINT('',(-0.685,7.3,5.));
#8803=CARTESIAN_POINT('Origin',(0.,8.5,5.));
#8804=CARTESIAN_POINT('Origin',(0.,7.3,5.));
#8805=CARTESIAN_POINT('',(-0.46,7.3,5.));
#8806=CARTESIAN_POINT('Origin',(0.,7.3,5.));
#8807=CARTESIAN_POINT('Origin',(0.,5.4,5.));
#8808=CARTESIAN_POINT('',(-1.065,5.5,5.));
#8809=CARTESIAN_POINT('Origin',(0.,5.5,5.));
#8810=CARTESIAN_POINT('',(-1.065,7.,5.));
#8811=CARTESIAN_POINT('',(-1.065,5.4,5.));
#8812=CARTESIAN_POINT('Origin',(0.,7.,5.));
#8813=CARTESIAN_POINT('Origin',(0.,7.,5.));
#8814=CARTESIAN_POINT('',(-0.46,7.,5.));
#8815=CARTESIAN_POINT('Origin',(0.,7.,5.));
#8816=CARTESIAN_POINT('Origin',(0.,5.5,5.));
#8817=CARTESIAN_POINT('',(-0.46,5.5,5.));
#8818=CARTESIAN_POINT('Origin',(0.,5.5,5.));
#8819=CARTESIAN_POINT('',(-1.5,8.5,5.));
#8820=CARTESIAN_POINT('Origin',(0.,8.5,5.));
#8821=CARTESIAN_POINT('',(-1.5,5.5,5.));
#8822=CARTESIAN_POINT('',(-1.5,5.5,5.));
#8823=CARTESIAN_POINT('Origin',(0.,5.5,5.));
#8824=CARTESIAN_POINT('Origin',(0.,8.5,5.));
#8825=CARTESIAN_POINT('Origin',(0.,5.5,5.));
#8826=CARTESIAN_POINT('',(0.,0.,0.));
#8827=CARTESIAN_POINT('Origin',(-4.5,8.5,3.));
#8828=CARTESIAN_POINT('',(-4.4,8.5,3.33));
#8829=CARTESIAN_POINT('Origin',(-4.4,8.5,3.));
#8830=CARTESIAN_POINT('',(-3.8,8.5,3.33));
#8831=CARTESIAN_POINT('',(-4.5,8.5,3.33));
#8832=CARTESIAN_POINT('Origin',(-3.8,8.5,3.));
#8833=CARTESIAN_POINT('Origin',(-4.5,-13.5,7.));
#8834=CARTESIAN_POINT('',(-4.4,-13.5,7.33));
#8835=CARTESIAN_POINT('Origin',(-4.4,-13.5,7.));
#8836=CARTESIAN_POINT('',(-3.8,-13.5,7.33));
#8837=CARTESIAN_POINT('',(-4.5,-13.5,7.33));
#8838=CARTESIAN_POINT('Origin',(-3.8,-13.5,7.));
#8839=CARTESIAN_POINT('Origin',(-4.5,-13.5,3.));
#8840=CARTESIAN_POINT('',(-4.4,-13.5,3.33));
#8841=CARTESIAN_POINT('Origin',(-4.4,-13.5,3.));
#8842=CARTESIAN_POINT('',(-3.8,-13.5,3.33));
#8843=CARTESIAN_POINT('',(-4.5,-13.5,3.33));
#8844=CARTESIAN_POINT('Origin',(-3.8,-13.5,3.));
#8845=CARTESIAN_POINT('Origin',(-4.5,8.5,7.));
#8846=CARTESIAN_POINT('',(-4.4,8.5,7.33));
#8847=CARTESIAN_POINT('Origin',(-4.4,8.5,7.));
#8848=CARTESIAN_POINT('',(-3.8,8.5,7.33));
#8849=CARTESIAN_POINT('',(-4.5,8.5,7.33));
#8850=CARTESIAN_POINT('Origin',(-3.8,8.5,7.));
#8851=CARTESIAN_POINT('Origin',(-4.5,-12.4,5.));
#8852=CARTESIAN_POINT('',(-4.4,-12.4,5.7));
#8853=CARTESIAN_POINT('Origin',(-4.4,-12.4,5.));
#8854=CARTESIAN_POINT('',(-3.5,-12.4,5.7));
#8855=CARTESIAN_POINT('',(-4.5,-12.4,5.7));
#8856=CARTESIAN_POINT('Origin',(-3.5,-12.4,5.));
#8857=CARTESIAN_POINT('Origin',(-3.8,-12.4,5.));
#8858=CARTESIAN_POINT('',(-3.5,-12.4,6.1));
#8859=CARTESIAN_POINT('Origin',(-3.5,-12.4,5.));
#8860=CARTESIAN_POINT('',(-3.8,-12.4,6.1));
#8861=CARTESIAN_POINT('',(-3.8,-12.4,6.1));
#8862=CARTESIAN_POINT('Origin',(-3.8,-12.4,5.));
#8863=CARTESIAN_POINT('Origin',(-3.5,-12.4,5.));
#8864=CARTESIAN_POINT('Origin',(2.2,7.,3.9));
#8865=CARTESIAN_POINT('',(1.95,7.,3.9));
#8866=CARTESIAN_POINT('Origin',(2.2,7.,3.9));
#8867=CARTESIAN_POINT('',(1.95,7.,4.95));
#8868=CARTESIAN_POINT('',(1.95,7.,3.9));
#8869=CARTESIAN_POINT('Origin',(2.2,7.,4.95));
#8870=CARTESIAN_POINT('Origin',(2.2,7.,3.9));
#8871=CARTESIAN_POINT('Origin',(2.2,7.,5.05));
#8872=CARTESIAN_POINT('',(1.87,7.,5.05));
#8873=CARTESIAN_POINT('Origin',(2.2,7.,5.05));
#8874=CARTESIAN_POINT('',(1.87,7.,7.));
#8875=CARTESIAN_POINT('',(1.87,7.,5.05));
#8876=CARTESIAN_POINT('Origin',(2.2,7.,7.));
#8877=CARTESIAN_POINT('Origin',(3.1,6.4,4.95));
#8878=CARTESIAN_POINT('',(3.,7.5,4.95));
#8879=CARTESIAN_POINT('',(3.,6.5,4.95));
#8880=CARTESIAN_POINT('',(3.,6.45,4.95));
#8881=CARTESIAN_POINT('',(1.50917195839308,7.5,4.95));
#8882=CARTESIAN_POINT('',(1.35,7.5,4.95));
#8883=CARTESIAN_POINT('',(1.50917195839308,6.5,4.95));
#8884=CARTESIAN_POINT('',(1.50917195839308,6.4,4.95));
#8885=CARTESIAN_POINT('',(1.35,6.5,4.95));
#8886=CARTESIAN_POINT('Origin',(0.,6.4,5.05));
#8887=CARTESIAN_POINT('',(3.,6.5,5.05));
#8888=CARTESIAN_POINT('',(3.,7.5,5.05));
#8889=CARTESIAN_POINT('',(3.,6.45,5.05));
#8890=CARTESIAN_POINT('',(1.50917195839308,6.5,5.05));
#8891=CARTESIAN_POINT('',(-0.2,6.5,5.05));
#8892=CARTESIAN_POINT('',(1.50917195839308,7.5,5.05));
#8893=CARTESIAN_POINT('',(1.50917195839308,6.4,5.05));
#8894=CARTESIAN_POINT('',(-0.2,7.5,5.05));
#8895=CARTESIAN_POINT('Origin',(-0.4,7.5,5.));
#8896=CARTESIAN_POINT('',(3.,7.5,3.));
#8897=CARTESIAN_POINT('',(3.,7.5,3.));
#8898=CARTESIAN_POINT('',(-3.8,7.5,3.));
#8899=CARTESIAN_POINT('',(-3.8,7.5,3.));
#8900=CARTESIAN_POINT('',(-3.8,7.5,7.));
#8901=CARTESIAN_POINT('',(-3.8,7.5,3.5));
#8902=CARTESIAN_POINT('',(3.,7.5,7.));
#8903=CARTESIAN_POINT('',(3.,7.5,7.));
#8904=CARTESIAN_POINT('',(3.,7.5,3.));
#8905=CARTESIAN_POINT('Origin',(0.,7.5,5.));
#8906=CARTESIAN_POINT('Origin',(0.,6.4,5.));
#8907=CARTESIAN_POINT('Origin',(0.,6.5,5.));
#8908=CARTESIAN_POINT('Origin',(3.,6.5,7.));
#8909=CARTESIAN_POINT('',(3.,6.5,7.));
#8910=CARTESIAN_POINT('',(3.,6.5,7.));
#8911=CARTESIAN_POINT('',(3.,6.5,3.));
#8912=CARTESIAN_POINT('Origin',(3.,6.5,3.));
#8913=CARTESIAN_POINT('',(-3.8,6.5,3.));
#8914=CARTESIAN_POINT('',(3.,6.5,3.));
#8915=CARTESIAN_POINT('',(-3.8,6.5,3.));
#8916=CARTESIAN_POINT('',(-3.8,-4.,3.));
#8917=CARTESIAN_POINT('',(3.,6.5,3.));
#8918=CARTESIAN_POINT('Origin',(3.,6.5,7.));
#8919=CARTESIAN_POINT('',(3.,6.5,3.));
#8920=CARTESIAN_POINT('Origin',(-3.8,6.5,7.));
#8921=CARTESIAN_POINT('',(-3.8,6.5,7.));
#8922=CARTESIAN_POINT('',(3.,6.5,7.));
#8923=CARTESIAN_POINT('',(-3.8,-4.,7.));
#8924=CARTESIAN_POINT('Origin',(-0.4,6.5,5.));
#8925=CARTESIAN_POINT('',(-3.8,6.5,3.5));
#8926=CARTESIAN_POINT('Origin',(2.2,-7.,3.9));
#8927=CARTESIAN_POINT('',(1.95,-7.,3.9));
#8928=CARTESIAN_POINT('Origin',(2.2,-7.,3.9));
#8929=CARTESIAN_POINT('',(1.95,-7.,4.95));
#8930=CARTESIAN_POINT('',(1.95,-7.,3.9));
#8931=CARTESIAN_POINT('Origin',(2.2,-7.,4.95));
#8932=CARTESIAN_POINT('Origin',(2.2,-7.,3.9));
#8933=CARTESIAN_POINT('Origin',(2.2,-7.,5.05));
#8934=CARTESIAN_POINT('',(1.87,-7.,5.05));
#8935=CARTESIAN_POINT('Origin',(2.2,-7.,5.05));
#8936=CARTESIAN_POINT('',(1.87,-7.,7.));
#8937=CARTESIAN_POINT('',(1.87,-7.,5.05));
#8938=CARTESIAN_POINT('Origin',(2.2,-7.,7.));
#8939=CARTESIAN_POINT('Origin',(3.1,-7.6,4.95));
#8940=CARTESIAN_POINT('',(3.,-6.5,4.95));
#8941=CARTESIAN_POINT('',(3.,-7.5,4.95));
#8942=CARTESIAN_POINT('',(3.,-7.55,4.95));
#8943=CARTESIAN_POINT('',(1.50917195839308,-6.5,4.95));
#8944=CARTESIAN_POINT('',(1.35,-6.5,4.95));
#8945=CARTESIAN_POINT('',(1.50917195839308,-7.5,4.95));
#8946=CARTESIAN_POINT('',(1.50917195839308,-7.6,4.95));
#8947=CARTESIAN_POINT('',(1.35,-7.5,4.95));
#8948=CARTESIAN_POINT('Origin',(0.,-7.6,5.05));
#8949=CARTESIAN_POINT('',(3.,-7.5,5.05));
#8950=CARTESIAN_POINT('',(3.,-6.5,5.05));
#8951=CARTESIAN_POINT('',(3.,-7.55,5.05));
#8952=CARTESIAN_POINT('',(1.50917195839308,-7.5,5.05));
#8953=CARTESIAN_POINT('',(-0.2,-7.5,5.05));
#8954=CARTESIAN_POINT('',(1.50917195839308,-6.5,5.05));
#8955=CARTESIAN_POINT('',(1.50917195839308,-7.6,5.05));
#8956=CARTESIAN_POINT('',(-0.2,-6.5,5.05));
#8957=CARTESIAN_POINT('Origin',(-0.4,-6.5,5.));
#8958=CARTESIAN_POINT('',(3.,-6.5,3.));
#8959=CARTESIAN_POINT('',(3.,-6.5,3.));
#8960=CARTESIAN_POINT('',(-3.8,-6.5,3.));
#8961=CARTESIAN_POINT('',(-3.8,-6.5,3.));
#8962=CARTESIAN_POINT('',(-3.8,-6.5,7.));
#8963=CARTESIAN_POINT('',(-3.8,-6.5,3.5));
#8964=CARTESIAN_POINT('',(3.,-6.5,7.));
#8965=CARTESIAN_POINT('',(3.,-6.5,7.));
#8966=CARTESIAN_POINT('',(3.,-6.5,3.));
#8967=CARTESIAN_POINT('Origin',(0.,-6.5,5.));
#8968=CARTESIAN_POINT('Origin',(0.,-7.6,5.));
#8969=CARTESIAN_POINT('Origin',(0.,-7.5,5.));
#8970=CARTESIAN_POINT('Origin',(3.,-7.5,7.));
#8971=CARTESIAN_POINT('',(3.,-7.5,7.));
#8972=CARTESIAN_POINT('',(3.,-7.5,7.));
#8973=CARTESIAN_POINT('',(3.,-7.5,3.));
#8974=CARTESIAN_POINT('Origin',(3.,-7.5,3.));
#8975=CARTESIAN_POINT('',(-3.8,-7.5,3.));
#8976=CARTESIAN_POINT('',(3.,-7.5,3.));
#8977=CARTESIAN_POINT('',(-3.8,-7.5,3.));
#8978=CARTESIAN_POINT('',(-3.8,-11.,3.));
#8979=CARTESIAN_POINT('',(3.,-7.5,3.));
#8980=CARTESIAN_POINT('Origin',(3.,-7.5,7.));
#8981=CARTESIAN_POINT('',(3.,-7.5,3.));
#8982=CARTESIAN_POINT('Origin',(-3.8,-7.5,7.));
#8983=CARTESIAN_POINT('',(-3.8,-7.5,7.));
#8984=CARTESIAN_POINT('',(3.,-7.5,7.));
#8985=CARTESIAN_POINT('',(-3.8,-11.,7.));
#8986=CARTESIAN_POINT('Origin',(-0.4,-7.5,5.));
#8987=CARTESIAN_POINT('',(-3.8,-7.5,3.5));
#8988=CARTESIAN_POINT('Origin',(-3.8,9.5,2.));
#8989=CARTESIAN_POINT('',(-3.8,9.5,2.));
#8990=CARTESIAN_POINT('',(-4.4,9.5,2.));
#8991=CARTESIAN_POINT('',(-3.8,9.5,2.));
#8992=CARTESIAN_POINT('',(-4.4,9.5,8.));
#8993=CARTESIAN_POINT('',(-4.4,9.5,2.));
#8994=CARTESIAN_POINT('',(-3.8,9.5,8.));
#8995=CARTESIAN_POINT('',(-3.8,9.5,8.));
#8996=CARTESIAN_POINT('',(-3.8,9.5,2.));
#8997=CARTESIAN_POINT('Origin',(-3.8,-14.5,2.));
#8998=CARTESIAN_POINT('',(-3.8,-14.5,2.));
#8999=CARTESIAN_POINT('',(-3.8,-14.5,2.));
#9000=CARTESIAN_POINT('',(-3.8,-14.5,8.));
#9001=CARTESIAN_POINT('',(-3.8,-14.5,8.));
#9002=CARTESIAN_POINT('',(-3.8,-14.5,2.));
#9003=CARTESIAN_POINT('Origin',(-4.4,-14.5,2.));
#9004=CARTESIAN_POINT('',(-4.4,-14.5,2.));
#9005=CARTESIAN_POINT('',(-4.4,-14.5,2.));
#9006=CARTESIAN_POINT('',(-4.4,-14.5,8.));
#9007=CARTESIAN_POINT('',(-4.4,-14.5,8.));
#9008=CARTESIAN_POINT('',(-4.4,-14.5,2.));
#9009=CARTESIAN_POINT('Origin',(-4.4,9.5,2.));
#9010=CARTESIAN_POINT('',(-4.4,9.5,2.));
#9011=CARTESIAN_POINT('',(-4.4,9.5,8.));
#9012=CARTESIAN_POINT('Origin',(-4.1,-2.5,8.));
#9013=CARTESIAN_POINT('Origin',(-4.1,-2.5,2.));
#9014=CARTESIAN_POINT('',(0.,0.,0.));
#9015=CARTESIAN_POINT('Origin',(-5.1,-12.4,5.));
#9016=CARTESIAN_POINT('',(-5.,-12.4,5.57));
#9017=CARTESIAN_POINT('Origin',(-5.,-12.4,5.));
#9018=CARTESIAN_POINT('',(-4.4,-12.4,5.57));
#9019=CARTESIAN_POINT('',(-5.1,-12.4,5.57));
#9020=CARTESIAN_POINT('Origin',(-4.4,-12.4,5.));
#9021=CARTESIAN_POINT('Origin',(-5.,-12.9484827557301,4.05));
#9022=CARTESIAN_POINT('',(-5.,-12.9484827557301,4.05));
#9023=CARTESIAN_POINT('',(-5.,-11.8515172442699,4.05));
#9024=CARTESIAN_POINT('',(-5.,-12.9484827557301,4.05));
#9025=CARTESIAN_POINT('',(-4.4,-11.8515172442699,4.05));
#9026=CARTESIAN_POINT('',(-5.,-11.8515172442699,4.05));
#9027=CARTESIAN_POINT('',(-4.4,-12.9484827557301,4.05));
#9028=CARTESIAN_POINT('',(-4.4,-12.9484827557301,4.05));
#9029=CARTESIAN_POINT('',(-5.,-12.9484827557301,4.05));
#9030=CARTESIAN_POINT('Origin',(-5.,-13.4969655114603,5.));
#9031=CARTESIAN_POINT('',(-5.,-13.4969655114603,5.));
#9032=CARTESIAN_POINT('',(-5.,-13.4969655114603,5.));
#9033=CARTESIAN_POINT('',(-4.4,-13.4969655114603,5.));
#9034=CARTESIAN_POINT('',(-4.4,-13.4969655114603,5.));
#9035=CARTESIAN_POINT('',(-5.,-13.4969655114603,5.));
#9036=CARTESIAN_POINT('Origin',(-5.,-12.9484827557301,5.95));
#9037=CARTESIAN_POINT('',(-5.,-12.9484827557301,5.95));
#9038=CARTESIAN_POINT('',(-5.,-12.9484827557301,5.95));
#9039=CARTESIAN_POINT('',(-4.4,-12.9484827557301,5.95));
#9040=CARTESIAN_POINT('',(-4.4,-12.9484827557301,5.95));
#9041=CARTESIAN_POINT('',(-5.,-12.9484827557301,5.95));
#9042=CARTESIAN_POINT('Origin',(-5.,-11.8515172442699,5.95));
#9043=CARTESIAN_POINT('',(-5.,-11.8515172442699,5.95));
#9044=CARTESIAN_POINT('',(-5.,-11.8515172442699,5.95));
#9045=CARTESIAN_POINT('',(-4.4,-11.8515172442699,5.95));
#9046=CARTESIAN_POINT('',(-4.4,-11.8515172442699,5.95));
#9047=CARTESIAN_POINT('',(-5.,-11.8515172442699,5.95));
#9048=CARTESIAN_POINT('Origin',(-5.,-11.3030344885397,5.));
#9049=CARTESIAN_POINT('',(-5.,-11.3030344885397,5.));
#9050=CARTESIAN_POINT('',(-5.,-11.3030344885397,5.));
#9051=CARTESIAN_POINT('',(-4.4,-11.3030344885397,5.));
#9052=CARTESIAN_POINT('',(-4.4,-11.3030344885397,5.));
#9053=CARTESIAN_POINT('',(-5.,-11.3030344885397,5.));
#9054=CARTESIAN_POINT('Origin',(-5.,-11.8515172442699,4.05));
#9055=CARTESIAN_POINT('',(-5.,-11.8515172442699,4.05));
#9056=CARTESIAN_POINT('',(-4.4,-11.8515172442699,4.05));
#9057=CARTESIAN_POINT('Origin',(-4.4,-12.4,5.));
#9058=CARTESIAN_POINT('Origin',(-5.,-12.4,5.));
#9059=CARTESIAN_POINT('',(0.,0.,0.));
#9060=CARTESIAN_POINT('Origin',(0.19,11.,5.));
#9061=CARTESIAN_POINT('',(-0.19,11.,5.));
#9062=CARTESIAN_POINT('Origin',(0.,11.,5.));
#9063=CARTESIAN_POINT('',(-0.125,11.,5.));
#9064=CARTESIAN_POINT('Origin',(0.,11.,5.));
#9065=CARTESIAN_POINT('Origin',(0.,10.8,5.));
#9066=CARTESIAN_POINT('',(-0.22,10.6,5.));
#9067=CARTESIAN_POINT('Origin',(0.,10.6,5.));
#9068=CARTESIAN_POINT('',(-0.205,10.8,5.));
#9069=CARTESIAN_POINT('Origin',(0.19,10.6,5.));
#9070=CARTESIAN_POINT('',(-0.19,10.6,5.));
#9071=CARTESIAN_POINT('Origin',(0.,10.6,5.));
#9072=CARTESIAN_POINT('Origin',(0.,10.5,5.));
#9073=CARTESIAN_POINT('',(-0.19,10.4,5.));
#9074=CARTESIAN_POINT('Origin',(0.,10.4,5.));
#9075=CARTESIAN_POINT('',(-0.19,10.5,5.));
#9076=CARTESIAN_POINT('Origin',(0.,10.2,5.));
#9077=CARTESIAN_POINT('',(-0.22,10.,5.));
#9078=CARTESIAN_POINT('Origin',(0.,10.,5.));
#9079=CARTESIAN_POINT('',(-0.205,10.2,5.));
#9080=CARTESIAN_POINT('Origin',(0.19,10.,5.));
#9081=CARTESIAN_POINT('',(-0.19,10.,5.));
#9082=CARTESIAN_POINT('Origin',(0.,10.,5.));
#9083=CARTESIAN_POINT('Origin',(0.,9.9,5.));
#9084=CARTESIAN_POINT('',(-0.19,9.8,5.));
#9085=CARTESIAN_POINT('Origin',(0.,9.8,5.));
#9086=CARTESIAN_POINT('',(-0.19,9.9,5.));
#9087=CARTESIAN_POINT('Origin',(0.,9.6,5.));
#9088=CARTESIAN_POINT('',(-0.22,9.4,5.));
#9089=CARTESIAN_POINT('Origin',(0.,9.4,5.));
#9090=CARTESIAN_POINT('',(-0.205,9.6,5.));
#9091=CARTESIAN_POINT('Origin',(0.19,9.4,5.));
#9092=CARTESIAN_POINT('',(-0.19,9.4,5.));
#9093=CARTESIAN_POINT('Origin',(0.,9.4,5.));
#9094=CARTESIAN_POINT('Origin',(0.,9.2,5.));
#9095=CARTESIAN_POINT('',(-0.19,9.,5.));
#9096=CARTESIAN_POINT('Origin',(0.,9.,5.));
#9097=CARTESIAN_POINT('',(-0.19,9.2,5.));
#9098=CARTESIAN_POINT('Origin',(0.,10.,5.));
#9099=CARTESIAN_POINT('',(-0.125,7.3,5.));
#9100=CARTESIAN_POINT('Origin',(0.,7.3,5.));
#9101=CARTESIAN_POINT('',(-0.125,10.,5.));
#9102=CARTESIAN_POINT('Origin',(0.,8.5,5.));
#9103=CARTESIAN_POINT('',(-0.505181485540923,8.5,4.125));
#9104=CARTESIAN_POINT('',(0.505181485540923,8.5,4.125));
#9105=CARTESIAN_POINT('',(-0.505181485540923,8.5,4.125));
#9106=CARTESIAN_POINT('',(1.01036297108185,8.5,5.));
#9107=CARTESIAN_POINT('',(0.505181485540923,8.5,4.125));
#9108=CARTESIAN_POINT('',(0.505181485540923,8.5,5.875));
#9109=CARTESIAN_POINT('',(1.01036297108185,8.5,5.));
#9110=CARTESIAN_POINT('',(-0.505181485540922,8.5,5.875));
#9111=CARTESIAN_POINT('',(0.505181485540923,8.5,5.875));
#9112=CARTESIAN_POINT('',(-1.01036297108185,8.5,5.));
#9113=CARTESIAN_POINT('',(-0.505181485540922,8.5,5.875));
#9114=CARTESIAN_POINT('',(-1.01036297108185,8.5,5.));
#9115=CARTESIAN_POINT('',(-0.685,8.5,5.));
#9116=CARTESIAN_POINT('Origin',(0.,8.5,5.));
#9117=CARTESIAN_POINT('Origin',(1.01036297108184,8.5,5.));
#9118=CARTESIAN_POINT('',(0.505181485540923,9.,4.125));
#9119=CARTESIAN_POINT('',(0.505181485540923,8.5,4.125));
#9120=CARTESIAN_POINT('',(1.01036297108185,9.,5.));
#9121=CARTESIAN_POINT('',(0.505181485540923,9.,4.125));
#9122=CARTESIAN_POINT('',(1.01036297108185,8.5,5.));
#9123=CARTESIAN_POINT('Origin',(0.505181485540923,8.5,5.875));
#9124=CARTESIAN_POINT('',(0.505181485540923,9.,5.875));
#9125=CARTESIAN_POINT('',(1.01036297108185,9.,5.));
#9126=CARTESIAN_POINT('',(0.505181485540923,8.5,5.875));
#9127=CARTESIAN_POINT('Origin',(-0.505181485540922,8.5,5.875));
#9128=CARTESIAN_POINT('',(-0.505181485540922,9.,5.875));
#9129=CARTESIAN_POINT('',(0.505181485540923,9.,5.875));
#9130=CARTESIAN_POINT('',(-0.505181485540922,8.5,5.875));
#9131=CARTESIAN_POINT('Origin',(-1.01036297108185,8.5,5.));
#9132=CARTESIAN_POINT('',(-1.01036297108185,9.,5.));
#9133=CARTESIAN_POINT('',(-0.505181485540922,9.,5.875));
#9134=CARTESIAN_POINT('',(-1.01036297108185,8.5,5.));
#9135=CARTESIAN_POINT('Origin',(-0.505181485540923,8.5,4.125));
#9136=CARTESIAN_POINT('',(-0.505181485540923,9.,4.125));
#9137=CARTESIAN_POINT('',(-1.01036297108185,9.,5.));
#9138=CARTESIAN_POINT('',(-0.505181485540923,8.5,4.125));
#9139=CARTESIAN_POINT('Origin',(0.505181485540923,8.5,4.125));
#9140=CARTESIAN_POINT('',(-0.505181485540923,9.,4.125));
#9141=CARTESIAN_POINT('Origin',(0.,9.,5.));
#9142=CARTESIAN_POINT('Origin',(0.,7.3,5.));
#9143=CARTESIAN_POINT('',(-0.685,7.3,5.));
#9144=CARTESIAN_POINT('',(-0.685,7.3,5.));
#9145=CARTESIAN_POINT('Origin',(0.,7.3,5.));
#9146=CARTESIAN_POINT('Origin',(0.,7.3,5.));
#9147=CARTESIAN_POINT('',(0.,0.,0.));
#9148=CARTESIAN_POINT('Origin',(-1.3,-1.,6.8));
#9149=CARTESIAN_POINT('',(-1.465,-1.,6.8));
#9150=CARTESIAN_POINT('Origin',(-1.3,-1.,6.8));
#9151=CARTESIAN_POINT('',(-1.465,-1.,7.5));
#9152=CARTESIAN_POINT('',(-1.465,-1.,6.8));
#9153=CARTESIAN_POINT('Origin',(-1.3,-1.,7.5));
#9154=CARTESIAN_POINT('Origin',(-1.3,-1.,6.8));
#9155=CARTESIAN_POINT('Origin',(1.3,-1.,6.8));
#9156=CARTESIAN_POINT('',(1.135,-1.,6.8));
#9157=CARTESIAN_POINT('Origin',(1.3,-1.,6.8));
#9158=CARTESIAN_POINT('',(1.135,-1.,7.5));
#9159=CARTESIAN_POINT('',(1.135,-1.,6.8));
#9160=CARTESIAN_POINT('Origin',(1.3,-1.,7.5));
#9161=CARTESIAN_POINT('Origin',(1.3,-1.,6.8));
#9162=CARTESIAN_POINT('Origin',(1.9,-3.1,3.1));
#9163=CARTESIAN_POINT('',(1.625,-3.,3.1));
#9164=CARTESIAN_POINT('Origin',(1.9,-3.,3.1));
#9165=CARTESIAN_POINT('',(1.625,-0.0249999999999999,3.1));
#9166=CARTESIAN_POINT('',(1.625,-3.1,3.1));
#9167=CARTESIAN_POINT('Origin',(1.9,-0.0249999999999999,3.1));
#9168=CARTESIAN_POINT('Origin',(-1.9,-3.1,6.9));
#9169=CARTESIAN_POINT('',(-2.175,-3.,6.9));
#9170=CARTESIAN_POINT('Origin',(-1.9,-3.,6.9));
#9171=CARTESIAN_POINT('',(-2.175,-0.0249999999999999,6.9));
#9172=CARTESIAN_POINT('',(-2.175,-3.1,6.9));
#9173=CARTESIAN_POINT('Origin',(-1.9,-0.0249999999999999,6.9));
#9174=CARTESIAN_POINT('Origin',(-1.9,-3.1,3.1));
#9175=CARTESIAN_POINT('',(-2.175,-3.,3.1));
#9176=CARTESIAN_POINT('Origin',(-1.9,-3.,3.1));
#9177=CARTESIAN_POINT('',(-2.175,-0.0249999999999999,3.1));
#9178=CARTESIAN_POINT('',(-2.175,-3.1,3.1));
#9179=CARTESIAN_POINT('Origin',(-1.9,-0.0249999999999999,3.1));
#9180=CARTESIAN_POINT('Origin',(1.9,-3.1,6.9));
#9181=CARTESIAN_POINT('',(1.625,-3.,6.9));
#9182=CARTESIAN_POINT('Origin',(1.9,-3.,6.9));
#9183=CARTESIAN_POINT('',(1.625,-0.0249999999999999,6.9));
#9184=CARTESIAN_POINT('',(1.625,-3.1,6.9));
#9185=CARTESIAN_POINT('Origin',(1.9,-0.0249999999999999,6.9));
#9186=CARTESIAN_POINT('Origin',(0.,0.,6.5));
#9187=CARTESIAN_POINT('',(0.699553428981661,-0.025,6.5));
#9188=CARTESIAN_POINT('',(0.699553428981661,-0.025,7.5));
#9189=CARTESIAN_POINT('',(0.699553428981661,-0.025,6.5));
#9190=CARTESIAN_POINT('',(-0.699553428981661,-0.025,6.5));
#9191=CARTESIAN_POINT('Origin',(0.,0.,6.5));
#9192=CARTESIAN_POINT('',(-0.699553428981661,-0.025,7.5));
#9193=CARTESIAN_POINT('',(-0.699553428981661,-0.025,6.5));
#9194=CARTESIAN_POINT('Origin',(0.,0.,7.5));
#9195=CARTESIAN_POINT('Origin',(0.,0.,6.5));
#9196=CARTESIAN_POINT('',(0.556214886532175,-0.025,6.5));
#9197=CARTESIAN_POINT('',(1.25,-0.025,6.5));
#9198=CARTESIAN_POINT('',(-0.556214886532175,-0.025,6.5));
#9199=CARTESIAN_POINT('Origin',(0.,0.,6.5));
#9200=CARTESIAN_POINT('',(1.25,-0.025,6.5));
#9201=CARTESIAN_POINT('Origin',(0.,-1.5125,7.5));
#9202=CARTESIAN_POINT('',(-2.5,-0.025,7.5));
#9203=CARTESIAN_POINT('',(2.5,-0.025,7.5));
#9204=CARTESIAN_POINT('',(-2.5,-3.,7.5));
#9205=CARTESIAN_POINT('',(-2.5,-0.025,7.5));
#9206=CARTESIAN_POINT('',(2.5,-3.,7.5));
#9207=CARTESIAN_POINT('',(-2.5,-3.,7.5));
#9208=CARTESIAN_POINT('',(2.5,-0.025,7.5));
#9209=CARTESIAN_POINT('',(2.5,-3.,7.5));
#9210=CARTESIAN_POINT('',(2.5,-0.025,7.5));
#9211=CARTESIAN_POINT('Origin',(0.,-3.1,5.));
#9212=CARTESIAN_POINT('',(-0.93,-3.,5.));
#9213=CARTESIAN_POINT('Origin',(0.,-3.,5.));
#9214=CARTESIAN_POINT('',(-0.93,-1.8,5.));
#9215=CARTESIAN_POINT('',(-0.93,-3.1,5.));
#9216=CARTESIAN_POINT('Origin',(0.,-1.8,5.));
#9217=CARTESIAN_POINT('Origin',(0.,-1.8,5.));
#9218=CARTESIAN_POINT('',(-1.3,-1.8,5.));
#9219=CARTESIAN_POINT('Origin',(0.,-1.8,5.));
#9220=CARTESIAN_POINT('',(-1.3,-1.,5.));
#9221=CARTESIAN_POINT('',(-1.3,-1.8,5.));
#9222=CARTESIAN_POINT('Origin',(0.,-1.,5.));
#9223=CARTESIAN_POINT('Origin',(0.,-1.,5.));
#9224=CARTESIAN_POINT('',(-1.52958336188405E-16,-1.,6.24899959967968));
#9225=CARTESIAN_POINT('Origin',(0.,-1.,5.));
#9226=CARTESIAN_POINT('Origin',(0.,-1.8,5.));
#9227=CARTESIAN_POINT('Origin',(0.,0.,5.));
#9228=CARTESIAN_POINT('Origin',(0.,-0.025,5.));
#9229=CARTESIAN_POINT('Origin',(2.5,-0.025,2.5));
#9230=CARTESIAN_POINT('',(2.5,-0.025,2.5));
#9231=CARTESIAN_POINT('',(2.5,-0.025,2.5));
#9232=CARTESIAN_POINT('',(-2.5,-0.025,2.5));
#9233=CARTESIAN_POINT('',(2.5,-0.025,2.5));
#9234=CARTESIAN_POINT('',(-2.5,-0.025,2.5));
#9235=CARTESIAN_POINT('Origin',(2.5,-3.,2.5));
#9236=CARTESIAN_POINT('',(2.5,-3.,2.5));
#9237=CARTESIAN_POINT('',(2.5,-3.,2.5));
#9238=CARTESIAN_POINT('',(2.5,-3.,2.5));
#9239=CARTESIAN_POINT('Origin',(-2.5,-3.,2.5));
#9240=CARTESIAN_POINT('',(-2.5,-3.,2.5));
#9241=CARTESIAN_POINT('',(-2.5,-3.,2.5));
#9242=CARTESIAN_POINT('',(-2.5,-3.,2.5));
#9243=CARTESIAN_POINT('Origin',(-2.5,-0.025,2.5));
#9244=CARTESIAN_POINT('',(-2.5,-0.025,2.5));
#9245=CARTESIAN_POINT('Origin',(0.,-1.5125,2.5));
#9246=CARTESIAN_POINT('',(0.,0.,0.));
#9247=CARTESIAN_POINT('Origin',(-1.3,1.,6.8));
#9248=CARTESIAN_POINT('',(-1.465,1.,6.8));
#9249=CARTESIAN_POINT('Origin',(-1.3,1.,6.8));
#9250=CARTESIAN_POINT('',(-1.465,1.,7.5));
#9251=CARTESIAN_POINT('',(-1.465,1.,6.8));
#9252=CARTESIAN_POINT('Origin',(-1.3,1.,7.5));
#9253=CARTESIAN_POINT('Origin',(-1.3,1.,6.8));
#9254=CARTESIAN_POINT('Origin',(1.3,1.,6.8));
#9255=CARTESIAN_POINT('',(1.135,1.,6.8));
#9256=CARTESIAN_POINT('Origin',(1.3,1.,6.8));
#9257=CARTESIAN_POINT('',(1.135,1.,7.5));
#9258=CARTESIAN_POINT('',(1.135,1.,6.8));
#9259=CARTESIAN_POINT('Origin',(1.3,1.,7.5));
#9260=CARTESIAN_POINT('Origin',(1.3,1.,6.8));
#9261=CARTESIAN_POINT('Origin',(1.9,-3.1,3.1));
#9262=CARTESIAN_POINT('',(1.625,0.0249999999999999,3.1));
#9263=CARTESIAN_POINT('Origin',(1.9,0.0249999999999999,3.1));
#9264=CARTESIAN_POINT('',(1.625,3.,3.1));
#9265=CARTESIAN_POINT('',(1.625,-3.1,3.1));
#9266=CARTESIAN_POINT('Origin',(1.9,3.,3.1));
#9267=CARTESIAN_POINT('Origin',(-1.9,-3.1,6.9));
#9268=CARTESIAN_POINT('',(-2.175,0.0249999999999999,6.9));
#9269=CARTESIAN_POINT('Origin',(-1.9,0.0249999999999999,6.9));
#9270=CARTESIAN_POINT('',(-2.175,3.,6.9));
#9271=CARTESIAN_POINT('',(-2.175,-3.1,6.9));
#9272=CARTESIAN_POINT('Origin',(-1.9,3.,6.9));
#9273=CARTESIAN_POINT('Origin',(-1.9,-3.1,3.1));
#9274=CARTESIAN_POINT('',(-2.175,0.0249999999999999,3.1));
#9275=CARTESIAN_POINT('Origin',(-1.9,0.0249999999999999,3.1));
#9276=CARTESIAN_POINT('',(-2.175,3.,3.1));
#9277=CARTESIAN_POINT('',(-2.175,-3.1,3.1));
#9278=CARTESIAN_POINT('Origin',(-1.9,3.,3.1));
#9279=CARTESIAN_POINT('Origin',(1.9,-3.1,6.9));
#9280=CARTESIAN_POINT('',(1.625,0.0249999999999999,6.9));
#9281=CARTESIAN_POINT('Origin',(1.9,0.0249999999999999,6.9));
#9282=CARTESIAN_POINT('',(1.625,3.,6.9));
#9283=CARTESIAN_POINT('',(1.625,-3.1,6.9));
#9284=CARTESIAN_POINT('Origin',(1.9,3.,6.9));
#9285=CARTESIAN_POINT('Origin',(0.,0.,6.5));
#9286=CARTESIAN_POINT('',(-0.699553428981661,0.025,6.5));
#9287=CARTESIAN_POINT('',(-0.699553428981661,0.025,7.5));
#9288=CARTESIAN_POINT('',(-0.699553428981661,0.025,6.5));
#9289=CARTESIAN_POINT('',(0.699553428981661,0.025,6.5));
#9290=CARTESIAN_POINT('Origin',(0.,0.,6.5));
#9291=CARTESIAN_POINT('',(0.699553428981661,0.025,7.5));
#9292=CARTESIAN_POINT('',(0.699553428981661,0.025,6.5));
#9293=CARTESIAN_POINT('Origin',(0.,0.,7.5));
#9294=CARTESIAN_POINT('Origin',(0.,0.,6.5));
#9295=CARTESIAN_POINT('',(-0.556214886532175,0.025,6.5));
#9296=CARTESIAN_POINT('',(-1.25,0.025,6.5));
#9297=CARTESIAN_POINT('',(0.556214886532175,0.025,6.5));
#9298=CARTESIAN_POINT('Origin',(0.,0.,6.5));
#9299=CARTESIAN_POINT('',(-1.25,0.025,6.5));
#9300=CARTESIAN_POINT('Origin',(0.,1.5125,7.5));
#9301=CARTESIAN_POINT('',(2.5,0.0249999999999999,7.5));
#9302=CARTESIAN_POINT('',(-2.5,0.025,7.5));
#9303=CARTESIAN_POINT('',(2.5,3.,7.5));
#9304=CARTESIAN_POINT('',(2.5,0.025,7.5));
#9305=CARTESIAN_POINT('',(-2.5,3.,7.5));
#9306=CARTESIAN_POINT('',(2.5,3.,7.5));
#9307=CARTESIAN_POINT('',(-2.5,0.0249999999999999,7.5));
#9308=CARTESIAN_POINT('',(-2.5,3.,7.5));
#9309=CARTESIAN_POINT('',(-2.5,0.025,7.5));
#9310=CARTESIAN_POINT('Origin',(0.,1.8,5.));
#9311=CARTESIAN_POINT('',(-0.93,1.8,5.));
#9312=CARTESIAN_POINT('Origin',(0.,1.8,5.));
#9313=CARTESIAN_POINT('',(-0.93,3.,5.));
#9314=CARTESIAN_POINT('',(-0.93,1.8,5.));
#9315=CARTESIAN_POINT('Origin',(0.,3.,5.));
#9316=CARTESIAN_POINT('Origin',(0.,1.,5.));
#9317=CARTESIAN_POINT('',(-1.3,1.,5.));
#9318=CARTESIAN_POINT('Origin',(0.,1.,5.));
#9319=CARTESIAN_POINT('',(-1.3,1.8,5.));
#9320=CARTESIAN_POINT('',(-1.3,1.,5.));
#9321=CARTESIAN_POINT('Origin',(0.,1.8,5.));
#9322=CARTESIAN_POINT('Origin',(0.,1.8,5.));
#9323=CARTESIAN_POINT('Origin',(0.,1.,5.));
#9324=CARTESIAN_POINT('',(-1.52958336188405E-16,1.,3.75100040032032));
#9325=CARTESIAN_POINT('Origin',(0.,1.,5.));
#9326=CARTESIAN_POINT('Origin',(0.,0.,5.));
#9327=CARTESIAN_POINT('Origin',(0.,0.025,5.));
#9328=CARTESIAN_POINT('Origin',(2.5,3.,2.5));
#9329=CARTESIAN_POINT('',(2.5,3.,2.5));
#9330=CARTESIAN_POINT('',(-2.5,3.,2.5));
#9331=CARTESIAN_POINT('',(2.5,3.,2.5));
#9332=CARTESIAN_POINT('',(-2.5,3.,2.5));
#9333=CARTESIAN_POINT('',(2.5,3.,2.5));
#9334=CARTESIAN_POINT('Origin',(2.5,0.025,2.5));
#9335=CARTESIAN_POINT('',(2.5,0.025,2.5));
#9336=CARTESIAN_POINT('',(2.5,0.025,2.5));
#9337=CARTESIAN_POINT('',(2.5,0.025,2.5));
#9338=CARTESIAN_POINT('Origin',(-2.5,0.025,2.5));
#9339=CARTESIAN_POINT('',(-2.5,0.0249999999999999,2.5));
#9340=CARTESIAN_POINT('',(-2.5,0.0249999999999999,2.5));
#9341=CARTESIAN_POINT('',(-2.5,0.025,2.5));
#9342=CARTESIAN_POINT('Origin',(-2.5,3.,2.5));
#9343=CARTESIAN_POINT('',(-2.5,3.,2.5));
#9344=CARTESIAN_POINT('Origin',(0.,1.5125,2.5));
#9345=CARTESIAN_POINT('',(0.,0.,0.));
#9346=CARTESIAN_POINT('Origin',(1.9,-0.1,3.1));
#9347=CARTESIAN_POINT('',(1.625,-0.025,3.1));
#9348=CARTESIAN_POINT('Origin',(1.9,-0.025,3.1));
#9349=CARTESIAN_POINT('',(1.625,0.025,3.1));
#9350=CARTESIAN_POINT('',(1.625,-0.1,3.1));
#9351=CARTESIAN_POINT('Origin',(1.9,0.025,3.1));
#9352=CARTESIAN_POINT('Origin',(-1.9,-0.1,6.9));
#9353=CARTESIAN_POINT('',(-2.175,-0.025,6.9));
#9354=CARTESIAN_POINT('Origin',(-1.9,-0.025,6.9));
#9355=CARTESIAN_POINT('',(-2.175,0.025,6.9));
#9356=CARTESIAN_POINT('',(-2.175,-0.1,6.9));
#9357=CARTESIAN_POINT('Origin',(-1.9,0.025,6.9));
#9358=CARTESIAN_POINT('Origin',(-1.9,-0.1,3.1));
#9359=CARTESIAN_POINT('',(-2.175,-0.025,3.1));
#9360=CARTESIAN_POINT('Origin',(-1.9,-0.025,3.1));
#9361=CARTESIAN_POINT('',(-2.175,0.025,3.1));
#9362=CARTESIAN_POINT('',(-2.175,-0.1,3.1));
#9363=CARTESIAN_POINT('Origin',(-1.9,0.025,3.1));
#9364=CARTESIAN_POINT('Origin',(1.9,-0.1,6.9));
#9365=CARTESIAN_POINT('',(1.625,-0.025,6.9));
#9366=CARTESIAN_POINT('Origin',(1.9,-0.025,6.9));
#9367=CARTESIAN_POINT('',(1.625,0.025,6.9));
#9368=CARTESIAN_POINT('',(1.625,-0.1,6.9));
#9369=CARTESIAN_POINT('Origin',(1.9,0.025,6.9));
#9370=CARTESIAN_POINT('Origin',(-0.7,-0.1,6.5));
#9371=CARTESIAN_POINT('',(-0.7,-0.025,6.5));
#9372=CARTESIAN_POINT('',(-0.7,-0.025,7.5));
#9373=CARTESIAN_POINT('',(-0.7,-0.025,5.75));
#9374=CARTESIAN_POINT('',(-0.7,0.025,6.5));
#9375=CARTESIAN_POINT('',(-0.7,-0.1,6.5));
#9376=CARTESIAN_POINT('',(-0.7,0.025,7.5));
#9377=CARTESIAN_POINT('',(-0.7,0.025,5.75));
#9378=CARTESIAN_POINT('',(-0.7,-0.0625,7.5));
#9379=CARTESIAN_POINT('Origin',(0.7,-0.1,6.5));
#9380=CARTESIAN_POINT('',(0.7,-0.025,6.5));
#9381=CARTESIAN_POINT('',(0.556776436283003,-0.025,6.5));
#9382=CARTESIAN_POINT('',(0.35,-0.025,6.5));
#9383=CARTESIAN_POINT('',(0.7,0.025,6.5));
#9384=CARTESIAN_POINT('',(0.7,-0.1,6.5));
#9385=CARTESIAN_POINT('',(0.556776436283003,0.025,6.5));
#9386=CARTESIAN_POINT('',(0.35,0.025,6.5));
#9387=CARTESIAN_POINT('',(0.556776436283003,-0.1,6.5));
#9388=CARTESIAN_POINT('Origin',(0.7,-0.1,6.5));
#9389=CARTESIAN_POINT('',(-0.556776436283003,-0.025,6.5));
#9390=CARTESIAN_POINT('',(0.35,-0.025,6.5));
#9391=CARTESIAN_POINT('',(-0.556776436283003,0.025,6.5));
#9392=CARTESIAN_POINT('',(-0.556776436283003,-0.1,6.5));
#9393=CARTESIAN_POINT('',(0.35,0.025,6.5));
#9394=CARTESIAN_POINT('Origin',(0.7,-0.1,7.6));
#9395=CARTESIAN_POINT('',(0.7,-0.025,7.5));
#9396=CARTESIAN_POINT('',(0.7,-0.025,6.3));
#9397=CARTESIAN_POINT('',(0.7,0.025,7.5));
#9398=CARTESIAN_POINT('',(0.7,-0.0625,7.5));
#9399=CARTESIAN_POINT('',(0.7,0.025,6.3));
#9400=CARTESIAN_POINT('Origin',(0.,0.025,5.));
#9401=CARTESIAN_POINT('Origin',(0.,0.025,5.));
#9402=CARTESIAN_POINT('',(2.5,0.025,7.5));
#9403=CARTESIAN_POINT('',(2.5,0.025,7.5));
#9404=CARTESIAN_POINT('',(2.5,0.025,2.5));
#9405=CARTESIAN_POINT('',(2.5,0.025,2.5));
#9406=CARTESIAN_POINT('',(-2.5,0.025,2.5));
#9407=CARTESIAN_POINT('',(-2.5,0.025,2.5));
#9408=CARTESIAN_POINT('',(-2.5,0.025,7.5));
#9409=CARTESIAN_POINT('',(-2.5,0.025,7.5));
#9410=CARTESIAN_POINT('',(2.5,0.025,7.5));
#9411=CARTESIAN_POINT('Origin',(-2.5,-0.025,7.5));
#9412=CARTESIAN_POINT('',(2.5,-0.025,7.5));
#9413=CARTESIAN_POINT('',(2.5,-0.025,7.5));
#9414=CARTESIAN_POINT('',(2.5,-0.025,7.5));
#9415=CARTESIAN_POINT('Origin',(-2.5,-0.025,7.5));
#9416=CARTESIAN_POINT('',(-2.5,-0.025,7.5));
#9417=CARTESIAN_POINT('',(-2.5,-0.025,7.5));
#9418=CARTESIAN_POINT('',(2.5,-0.025,7.5));
#9419=CARTESIAN_POINT('Origin',(0.,-0.1,5.));
#9420=CARTESIAN_POINT('Origin',(0.,-0.025,5.));
#9421=CARTESIAN_POINT('Origin',(-2.5,-0.025,2.5));
#9422=CARTESIAN_POINT('',(-2.5,-0.025,2.5));
#9423=CARTESIAN_POINT('',(-2.5,-0.025,7.5));
#9424=CARTESIAN_POINT('',(-2.5,-0.025,2.5));
#9425=CARTESIAN_POINT('Origin',(2.5,-0.025,2.5));
#9426=CARTESIAN_POINT('',(2.5,-0.025,2.5));
#9427=CARTESIAN_POINT('',(-2.5,-0.025,2.5));
#9428=CARTESIAN_POINT('',(2.5,-0.025,2.5));
#9429=CARTESIAN_POINT('Origin',(2.5,-0.025,7.5));
#9430=CARTESIAN_POINT('',(2.5,-0.025,2.5));
#9431=CARTESIAN_POINT('Origin',(0.,-0.025,5.));
#9432=CARTESIAN_POINT('',(0.,0.,0.));
#9433=CARTESIAN_POINT('Origin',(0.,0.,7.5));
#9434=CARTESIAN_POINT('',(-1.2,-1.46957615897682E-16,7.5));
#9435=CARTESIAN_POINT('Origin',(0.,0.,7.5));
#9436=CARTESIAN_POINT('',(-0.7,-8.57252759403147E-17,7.5));
#9437=CARTESIAN_POINT('Origin',(0.,0.,7.5));
#9438=CARTESIAN_POINT('Origin',(0.,0.,7.5));
#9439=CARTESIAN_POINT('',(-1.2,-1.46957615897682E-16,8.));
#9440=CARTESIAN_POINT('Origin',(0.,0.,8.));
#9441=CARTESIAN_POINT('',(-1.2,-1.46957615897682E-16,7.5));
#9442=CARTESIAN_POINT('Origin',(0.,0.,8.));
#9443=CARTESIAN_POINT('',(-0.405,-4.95981953654678E-17,8.));
#9444=CARTESIAN_POINT('Origin',(0.,0.,8.));
#9445=CARTESIAN_POINT('Origin',(0.,0.,6.6));
#9446=CARTESIAN_POINT('',(-0.405,-4.95981953654678E-17,6.6));
#9447=CARTESIAN_POINT('',(-0.405,-4.95981953654678E-17,6.6));
#9448=CARTESIAN_POINT('Origin',(0.,0.,6.6));
#9449=CARTESIAN_POINT('Origin',(0.,0.,6.6));
#9450=CARTESIAN_POINT('',(-0.7,-8.57252759403147E-17,6.6));
#9451=CARTESIAN_POINT('',(-0.7,-8.57252759403147E-17,6.6));
#9452=CARTESIAN_POINT('Origin',(0.,0.,6.6));
#9453=CARTESIAN_POINT('Origin',(0.,0.,6.6));
#9454=CARTESIAN_POINT('',(0.,0.,0.));
#9455=CARTESIAN_POINT('Origin',(0.,0.,8.1));
#9456=CARTESIAN_POINT('',(-0.4,-4.89858719658941E-17,8.1));
#9457=CARTESIAN_POINT('Origin',(-0.5,-6.12323399573677E-17,8.1));
#9458=CARTESIAN_POINT('Origin',(0.,0.,8.1));
#9459=CARTESIAN_POINT('',(0.,0.,0.));
#9460=CARTESIAN_POINT('Origin',(0.,0.,7.9));
#9461=CARTESIAN_POINT('',(-0.61,-7.47034547479885E-17,8.));
#9462=CARTESIAN_POINT('Origin',(0.,0.,8.));
#9463=CARTESIAN_POINT('',(-0.61,-7.47034547479885E-17,8.3));
#9464=CARTESIAN_POINT('',(-0.61,-7.47034547479885E-17,7.9));
#9465=CARTESIAN_POINT('Origin',(0.,0.,8.3));
#9466=CARTESIAN_POINT('Origin',(0.,0.,8.3));
#9467=CARTESIAN_POINT('',(-0.405,4.95981953654678E-17,8.3));
#9468=CARTESIAN_POINT('Origin',(0.,0.,8.3));
#9469=CARTESIAN_POINT('Origin',(0.,0.,8.));
#9470=CARTESIAN_POINT('',(-0.405,-4.95981953654678E-17,8.7));
#9471=CARTESIAN_POINT('Origin',(0.,0.,8.7));
#9472=CARTESIAN_POINT('',(-0.405,-4.95981953654678E-17,8.));
#9473=CARTESIAN_POINT('Origin',(0.,0.,8.));
#9474=CARTESIAN_POINT('',(-1.,-1.22464679914735E-16,8.7));
#9475=CARTESIAN_POINT('Origin',(0.,0.,8.7));
#9476=CARTESIAN_POINT('',(-1.,-1.22464679914735E-16,8.));
#9477=CARTESIAN_POINT('',(-1.,-1.22464679914735E-16,8.));
#9478=CARTESIAN_POINT('Origin',(0.,0.,8.));
#9479=CARTESIAN_POINT('Origin',(0.,0.,8.7));
#9480=CARTESIAN_POINT('Origin',(0.,0.,8.));
#9481=CARTESIAN_POINT('',(0.,0.,0.));
#9482=CARTESIAN_POINT('Origin',(-1.1,-3.,8.1));
#9483=CARTESIAN_POINT('',(-1.4,-3.,8.1));
#9484=CARTESIAN_POINT('Origin',(-1.1,-3.,8.1));
#9485=CARTESIAN_POINT('',(-1.4,-3.,8.5));
#9486=CARTESIAN_POINT('',(-1.4,-3.,8.1));
#9487=CARTESIAN_POINT('Origin',(-1.1,-3.,8.5));
#9488=CARTESIAN_POINT('Origin',(-1.1,-3.,8.1));
#9489=CARTESIAN_POINT('Origin',(3.,1.1,8.1));
#9490=CARTESIAN_POINT('',(2.7,1.1,8.1));
#9491=CARTESIAN_POINT('Origin',(3.,1.1,8.1));
#9492=CARTESIAN_POINT('',(2.7,1.1,8.5));
#9493=CARTESIAN_POINT('',(2.7,1.1,8.1));
#9494=CARTESIAN_POINT('Origin',(3.,1.1,8.5));
#9495=CARTESIAN_POINT('Origin',(3.,1.1,8.1));
#9496=CARTESIAN_POINT('Origin',(1.3,-1.,7.9));
#9497=CARTESIAN_POINT('',(1.075,-1.,8.));
#9498=CARTESIAN_POINT('Origin',(1.3,-1.,8.));
#9499=CARTESIAN_POINT('',(1.075,-1.,8.5));
#9500=CARTESIAN_POINT('',(1.075,-1.,7.9));
#9501=CARTESIAN_POINT('Origin',(1.3,-1.,8.5));
#9502=CARTESIAN_POINT('Origin',(-1.3,1.,7.9));
#9503=CARTESIAN_POINT('',(-1.525,1.,8.));
#9504=CARTESIAN_POINT('Origin',(-1.3,1.,8.));
#9505=CARTESIAN_POINT('',(-1.525,1.,8.5));
#9506=CARTESIAN_POINT('',(-1.525,1.,7.9));
#9507=CARTESIAN_POINT('Origin',(-1.3,1.,8.5));
#9508=CARTESIAN_POINT('Origin',(-1.3,-1.,7.9));
#9509=CARTESIAN_POINT('',(-1.525,-1.,8.));
#9510=CARTESIAN_POINT('Origin',(-1.3,-1.,8.));
#9511=CARTESIAN_POINT('',(-1.525,-1.,8.5));
#9512=CARTESIAN_POINT('',(-1.525,-1.,7.9));
#9513=CARTESIAN_POINT('Origin',(-1.3,-1.,8.5));
#9514=CARTESIAN_POINT('Origin',(1.3,1.,7.9));
#9515=CARTESIAN_POINT('',(1.075,1.,8.));
#9516=CARTESIAN_POINT('Origin',(1.3,1.,8.));
#9517=CARTESIAN_POINT('',(1.075,1.,8.5));
#9518=CARTESIAN_POINT('',(1.075,1.,7.9));
#9519=CARTESIAN_POINT('Origin',(1.3,1.,8.5));
#9520=CARTESIAN_POINT('Origin',(0.,0.,7.9));
#9521=CARTESIAN_POINT('',(-1.01,-1.23689326713883E-16,8.));
#9522=CARTESIAN_POINT('Origin',(0.,0.,8.));
#9523=CARTESIAN_POINT('',(-1.01,1.23689326713883E-16,8.5));
#9524=CARTESIAN_POINT('',(-1.01,-1.23689326713883E-16,7.9));
#9525=CARTESIAN_POINT('Origin',(0.,0.,8.5));
#9526=CARTESIAN_POINT('Origin',(4.,1.5,8.));
#9527=CARTESIAN_POINT('',(4.,1.5,8.));
#9528=CARTESIAN_POINT('',(-2.5,1.5,8.));
#9529=CARTESIAN_POINT('',(4.,1.5,8.));
#9530=CARTESIAN_POINT('',(-2.5,1.5,8.5));
#9531=CARTESIAN_POINT('',(-2.5,1.5,8.));
#9532=CARTESIAN_POINT('',(4.,1.5,8.5));
#9533=CARTESIAN_POINT('',(4.,1.5,8.5));
#9534=CARTESIAN_POINT('',(4.,1.5,8.));
#9535=CARTESIAN_POINT('Origin',(4.,-4.,8.));
#9536=CARTESIAN_POINT('',(4.,-4.,8.));
#9537=CARTESIAN_POINT('',(4.,-4.,8.));
#9538=CARTESIAN_POINT('',(4.,-4.,8.5));
#9539=CARTESIAN_POINT('',(4.,-4.,8.5));
#9540=CARTESIAN_POINT('',(4.,-4.,8.));
#9541=CARTESIAN_POINT('Origin',(-2.5,-4.,8.));
#9542=CARTESIAN_POINT('',(-2.5,-4.,8.));
#9543=CARTESIAN_POINT('',(-2.5,-4.,8.));
#9544=CARTESIAN_POINT('',(-2.5,-4.,8.5));
#9545=CARTESIAN_POINT('',(-2.5,-4.,8.5));
#9546=CARTESIAN_POINT('',(-2.5,-4.,8.));
#9547=CARTESIAN_POINT('Origin',(-2.5,1.5,8.));
#9548=CARTESIAN_POINT('',(-2.5,1.5,8.));
#9549=CARTESIAN_POINT('',(-2.5,1.5,8.5));
#9550=CARTESIAN_POINT('Origin',(0.75,-1.25,8.5));
#9551=CARTESIAN_POINT('Origin',(0.75,-1.25,8.));
#9552=CARTESIAN_POINT('',(0.,0.,0.));
#9553=CARTESIAN_POINT('Origin',(0.,0.,5.));
#9554=CARTESIAN_POINT('',(-1.36919674566051E-16,-1.,6.11803398874989));
#9555=CARTESIAN_POINT('Origin',(0.,-1.,5.));
#9556=CARTESIAN_POINT('',(-0.75,-1.29903810567666,5.));
#9557=CARTESIAN_POINT('Origin',(0.,-1.29903810567666,5.));
#9558=CARTESIAN_POINT('Origin',(0.,-1.8,5.));
#9559=CARTESIAN_POINT('',(-0.75,-1.8,5.));
#9560=CARTESIAN_POINT('',(-0.75,-1.8,5.));
#9561=CARTESIAN_POINT('Origin',(0.,-1.8,5.));
#9562=CARTESIAN_POINT('Origin',(0.,-1.8,5.));
#9563=CARTESIAN_POINT('',(-1.3,-1.,5.));
#9564=CARTESIAN_POINT('Origin',(0.,-1.,5.));
#9565=CARTESIAN_POINT('',(-1.3,-1.8,5.));
#9566=CARTESIAN_POINT('',(-1.3,-1.8,5.));
#9567=CARTESIAN_POINT('Origin',(0.,-1.8,5.));
#9568=CARTESIAN_POINT('Origin',(0.,-1.,5.));
#9569=CARTESIAN_POINT('Origin',(0.,-1.8,5.));
#9570=CARTESIAN_POINT('',(0.,0.,0.));
#9571=CARTESIAN_POINT('Origin',(0.115470053837925,-0.5,-0.2));
#9572=CARTESIAN_POINT('',(0.23094010767585,-0.5,0.));
#9573=CARTESIAN_POINT('',(0.115470053837925,-0.5,-0.2));
#9574=CARTESIAN_POINT('',(0.23094010767585,-0.5,0.));
#9575=CARTESIAN_POINT('',(0.115470053837925,-0.8,-0.2));
#9576=CARTESIAN_POINT('',(0.115470053837925,-0.5,-0.2));
#9577=CARTESIAN_POINT('',(0.23094010767585,-0.8,0.));
#9578=CARTESIAN_POINT('',(0.23094010767585,-0.8,0.));
#9579=CARTESIAN_POINT('',(0.23094010767585,-0.5,0.));
#9580=CARTESIAN_POINT('Origin',(-0.115470053837925,-0.5,-0.2));
#9581=CARTESIAN_POINT('',(-0.115470053837925,-0.5,-0.2));
#9582=CARTESIAN_POINT('',(0.115470053837925,-0.5,-0.2));
#9583=CARTESIAN_POINT('',(-0.115470053837925,-0.8,-0.2));
#9584=CARTESIAN_POINT('',(-0.115470053837925,-0.5,-0.2));
#9585=CARTESIAN_POINT('',(0.115470053837925,-0.8,-0.2));
#9586=CARTESIAN_POINT('Origin',(-0.23094010767585,-0.5,-2.77555756156289E-17));
#9587=CARTESIAN_POINT('',(-0.23094010767585,-0.5,-2.82820063659975E-17));
#9588=CARTESIAN_POINT('',(-0.115470053837925,-0.5,-0.2));
#9589=CARTESIAN_POINT('',(-0.23094010767585,-0.8,-2.77555756156289E-17));
#9590=CARTESIAN_POINT('',(-0.23094010767585,-0.5,-2.82820063659975E-17));
#9591=CARTESIAN_POINT('',(-0.115470053837925,-0.8,-0.2));
#9592=CARTESIAN_POINT('Origin',(-0.115470053837925,-0.5,0.2));
#9593=CARTESIAN_POINT('',(-0.115470053837925,-0.5,0.2));
#9594=CARTESIAN_POINT('',(-0.23094010767585,-0.5,-2.82820063659975E-17));
#9595=CARTESIAN_POINT('',(-0.115470053837925,-0.8,0.2));
#9596=CARTESIAN_POINT('',(-0.115470053837925,-0.5,0.2));
#9597=CARTESIAN_POINT('',(-0.23094010767585,-0.8,-2.82820063659975E-17));
#9598=CARTESIAN_POINT('Origin',(0.115470053837925,-0.5,0.2));
#9599=CARTESIAN_POINT('',(0.115470053837925,-0.5,0.2));
#9600=CARTESIAN_POINT('',(-0.115470053837925,-0.5,0.2));
#9601=CARTESIAN_POINT('',(0.115470053837925,-0.8,0.2));
#9602=CARTESIAN_POINT('',(0.115470053837925,-0.5,0.2));
#9603=CARTESIAN_POINT('',(-0.115470053837925,-0.8,0.2));
#9604=CARTESIAN_POINT('Origin',(0.23094010767585,-0.5,0.));
#9605=CARTESIAN_POINT('',(0.115470053837925,-0.5,0.2));
#9606=CARTESIAN_POINT('',(0.115470053837925,-0.8,0.2));
#9607=CARTESIAN_POINT('Origin',(0.,-0.5,0.));
#9608=CARTESIAN_POINT('Origin',(0.,-0.8,0.));
#9609=CARTESIAN_POINT('Origin',(0.,-1.9,0.));
#9610=CARTESIAN_POINT('',(-0.25,-1.9,3.06161699786838E-17));
#9611=CARTESIAN_POINT('Origin',(0.,-1.9,0.));
#9612=CARTESIAN_POINT('',(-0.24505,-1.9,3.00099698131059E-17));
#9613=CARTESIAN_POINT('Origin',(0.,-1.9,0.));
#9614=CARTESIAN_POINT('Origin',(0.,-7.,0.));
#9615=CARTESIAN_POINT('',(-0.25,-7.,3.06161699786838E-17));
#9616=CARTESIAN_POINT('',(-0.25,-7.,3.06161699786838E-17));
#9617=CARTESIAN_POINT('Origin',(0.,-7.,0.));
#9618=CARTESIAN_POINT('Origin',(0.,-7.,0.));
#9619=CARTESIAN_POINT('Origin',(0.375,0.5,0.));
#9620=CARTESIAN_POINT('',(-0.375,0.5,-4.59242549680257E-17));
#9621=CARTESIAN_POINT('Origin',(0.,0.5,0.));
#9622=CARTESIAN_POINT('Origin',(0.,0.475,0.));
#9623=CARTESIAN_POINT('',(-0.425,0.45,-5.20474889637625E-17));
#9624=CARTESIAN_POINT('Origin',(0.,0.45,0.));
#9625=CARTESIAN_POINT('',(-0.4,0.475,-4.89858719658941E-17));
#9626=CARTESIAN_POINT('Origin',(0.,0.24,0.));
#9627=CARTESIAN_POINT('',(-0.425,0.0299999999999998,-5.20474889637625E-17));
#9628=CARTESIAN_POINT('Origin',(0.,0.0299999999999998,0.));
#9629=CARTESIAN_POINT('',(-0.425,0.24,-5.20474889637625E-17));
#9630=CARTESIAN_POINT('Origin',(0.,0.0150000000000001,0.));
#9631=CARTESIAN_POINT('',(-0.395,4.85722573273506E-17,-4.83735485663204E-17));
#9632=CARTESIAN_POINT('Origin',(0.,0.,0.));
#9633=CARTESIAN_POINT('',(-0.41,0.0150000000000001,-5.02105187650415E-17));
#9634=CARTESIAN_POINT('Origin',(0.27,0.,0.));
#9635=CARTESIAN_POINT('',(-0.27,0.,-3.30654635769785E-17));
#9636=CARTESIAN_POINT('Origin',(0.,0.,0.));
#9637=CARTESIAN_POINT('Origin',(0.,-0.02,0.));
#9638=CARTESIAN_POINT('',(-0.24505,-0.0498999999999999,3.00099698131059E-17));
#9639=CARTESIAN_POINT('Origin',(0.,-0.0498999999999999,0.));
#9640=CARTESIAN_POINT('',(-0.26,-0.02,-3.18408167778312E-17));
#9641=CARTESIAN_POINT('Origin',(0.,-0.995,0.));
#9642=CARTESIAN_POINT('',(-0.24505,-0.995,-3.00099698131059E-17));
#9643=CARTESIAN_POINT('',(0.,0.,0.));
#9644=CARTESIAN_POINT('Origin',(0.,0.09,0.));
#9645=CARTESIAN_POINT('',(-0.285,0.1,3.49024337756996E-17));
#9646=CARTESIAN_POINT('Origin',(0.,0.1,0.));
#9647=CARTESIAN_POINT('',(-0.265,0.08,-3.24531401774049E-17));
#9648=CARTESIAN_POINT('',(-0.275,0.09,3.36777869765522E-17));
#9649=CARTESIAN_POINT('Origin',(0.,0.08,0.));
#9650=CARTESIAN_POINT('Origin',(0.,0.,0.));
#9651=CARTESIAN_POINT('',(-0.265,0.,3.24531401774049E-17));
#9652=CARTESIAN_POINT('',(-0.265,0.,3.24531401774049E-17));
#9653=CARTESIAN_POINT('Origin',(0.,0.,0.));
#9654=CARTESIAN_POINT('Origin',(0.,0.1,0.));
#9655=CARTESIAN_POINT('',(-0.5,0.1,6.12323399573677E-17));
#9656=CARTESIAN_POINT('Origin',(0.,0.1,0.));
#9657=CARTESIAN_POINT('Origin',(0.,0.,0.));
#9658=CARTESIAN_POINT('',(-0.5,0.,6.12323399573677E-17));
#9659=CARTESIAN_POINT('',(-0.5,0.,6.12323399573677E-17));
#9660=CARTESIAN_POINT('Origin',(0.,0.,0.));
#9661=CARTESIAN_POINT('Origin',(0.,0.,0.));
#9662=CARTESIAN_POINT('',(0.,0.,0.));
#9663=CARTESIAN_POINT('Origin',(0.,0.0525042956467857,0.));
#9664=CARTESIAN_POINT('',(-0.230940107675851,0.0472735643746089,0.4));
#9665=CARTESIAN_POINT('',(0.23094010767585,0.0472735643746089,0.4));
#9666=CARTESIAN_POINT('Ctrl Pts',(-0.230940107675851,0.0472735643746089,
0.4));
#9667=CARTESIAN_POINT('Ctrl Pts',(1.11022302462516E-16,-0.0193931022920578,
0.4));
#9668=CARTESIAN_POINT('Ctrl Pts',(0.23094010767585,0.0472735643746089,0.4));
#9669=CARTESIAN_POINT('',(-0.461880215351701,0.0472735643746089,-5.6564012731995E-17));
#9670=CARTESIAN_POINT('Ctrl Pts',(-0.461880215351701,0.0472735643746089,
-5.6564012731995E-17));
#9671=CARTESIAN_POINT('Ctrl Pts',(-0.346410161513776,-0.0193931022920579,
0.2));
#9672=CARTESIAN_POINT('Ctrl Pts',(-0.230940107675851,0.0472735643746089,
0.4));
#9673=CARTESIAN_POINT('',(-0.38,-2.08166817117217E-17,-4.65365783675994E-17));
#9674=CARTESIAN_POINT('',(-0.47094010767585,0.0525042956467857,-5.7673529545534E-17));
#9675=CARTESIAN_POINT('Origin',(0.,0.,0.));
#9676=CARTESIAN_POINT('',(-0.23094010767585,0.0472735643746089,-0.4));
#9677=CARTESIAN_POINT('Ctrl Pts',(-0.23094010767585,0.0472735643746089,
-0.4));
#9678=CARTESIAN_POINT('Ctrl Pts',(-0.346410161513775,-0.0193931022920578,
-0.2));
#9679=CARTESIAN_POINT('Ctrl Pts',(-0.461880215351701,0.0472735643746089,
-5.6564012731995E-17));
#9680=CARTESIAN_POINT('',(0.23094010767585,0.0472735643746089,-0.4));
#9681=CARTESIAN_POINT('Ctrl Pts',(0.23094010767585,0.0472735643746089,-0.4));
#9682=CARTESIAN_POINT('Ctrl Pts',(0.,-0.0193931022920578,-0.4));
#9683=CARTESIAN_POINT('Ctrl Pts',(-0.23094010767585,0.0472735643746089,
-0.4));
#9684=CARTESIAN_POINT('',(0.461880215351701,0.0472735643746089,0.));
#9685=CARTESIAN_POINT('Ctrl Pts',(0.461880215351701,0.0472735643746089,
0.));
#9686=CARTESIAN_POINT('Ctrl Pts',(0.346410161513776,-0.019393102292058,
-0.2));
#9687=CARTESIAN_POINT('Ctrl Pts',(0.23094010767585,0.0472735643746089,-0.4));
#9688=CARTESIAN_POINT('Ctrl Pts',(0.23094010767585,0.0472735643746089,0.4));
#9689=CARTESIAN_POINT('Ctrl Pts',(0.346410161513776,-0.0193931022920577,
0.2));
#9690=CARTESIAN_POINT('Ctrl Pts',(0.461880215351701,0.0472735643746089,
0.));
#9691=CARTESIAN_POINT('Origin',(0.,0.417495704353214,0.));
#9692=CARTESIAN_POINT('',(-0.38,0.47,-4.65365783675994E-17));
#9693=CARTESIAN_POINT('Origin',(0.,0.47,0.));
#9694=CARTESIAN_POINT('',(-0.461880215351701,0.422726435625391,-5.6564012731995E-17));
#9695=CARTESIAN_POINT('',(-0.47094010767585,0.417495704353214,-5.7673529545534E-17));
#9696=CARTESIAN_POINT('',(-0.230940107675851,0.422726435625391,0.4));
#9697=CARTESIAN_POINT('Ctrl Pts',(-0.230940107675851,0.422726435625391,
0.4));
#9698=CARTESIAN_POINT('Ctrl Pts',(-0.346410161513776,0.489393102292058,
0.2));
#9699=CARTESIAN_POINT('Ctrl Pts',(-0.461880215351701,0.422726435625391,
-5.6564012731995E-17));
#9700=CARTESIAN_POINT('',(0.23094010767585,0.422726435625391,0.4));
#9701=CARTESIAN_POINT('Ctrl Pts',(0.23094010767585,0.422726435625391,0.4));
#9702=CARTESIAN_POINT('Ctrl Pts',(8.32667268468867E-17,0.489393102292058,
0.4));
#9703=CARTESIAN_POINT('Ctrl Pts',(-0.230940107675851,0.422726435625391,
0.4));
#9704=CARTESIAN_POINT('',(0.461880215351701,0.422726435625391,0.));
#9705=CARTESIAN_POINT('Ctrl Pts',(0.461880215351701,0.422726435625391,0.));
#9706=CARTESIAN_POINT('Ctrl Pts',(0.346410161513776,0.489393102292058,0.2));
#9707=CARTESIAN_POINT('Ctrl Pts',(0.23094010767585,0.422726435625391,0.4));
#9708=CARTESIAN_POINT('',(0.23094010767585,0.422726435625391,-0.4));
#9709=CARTESIAN_POINT('Ctrl Pts',(0.23094010767585,0.422726435625391,-0.4));
#9710=CARTESIAN_POINT('Ctrl Pts',(0.346410161513775,0.489393102292058,-0.2));
#9711=CARTESIAN_POINT('Ctrl Pts',(0.461880215351701,0.422726435625391,0.));
#9712=CARTESIAN_POINT('',(-0.23094010767585,0.422726435625391,-0.4));
#9713=CARTESIAN_POINT('Ctrl Pts',(-0.23094010767585,0.422726435625391,-0.4));
#9714=CARTESIAN_POINT('Ctrl Pts',(-5.55111512312578E-17,0.489393102292058,
-0.4));
#9715=CARTESIAN_POINT('Ctrl Pts',(0.23094010767585,0.422726435625391,-0.4));
#9716=CARTESIAN_POINT('Ctrl Pts',(-0.461880215351701,0.422726435625391,
-5.6564012731995E-17));
#9717=CARTESIAN_POINT('Ctrl Pts',(-0.346410161513776,0.489393102292058,
-0.2));
#9718=CARTESIAN_POINT('Ctrl Pts',(-0.23094010767585,0.422726435625391,-0.4));
#9719=CARTESIAN_POINT('Origin',(0.23094010767585,0.,-0.4));
#9720=CARTESIAN_POINT('',(-0.23094010767585,0.,-0.4));
#9721=CARTESIAN_POINT('',(0.23094010767585,0.,-0.4));
#9722=CARTESIAN_POINT('Origin',(-0.23094010767585,0.,-0.4));
#9723=CARTESIAN_POINT('',(-0.461880215351701,0.,-5.6564012731995E-17));
#9724=CARTESIAN_POINT('Origin',(-0.461880215351701,0.,-5.6564012731995E-17));
#9725=CARTESIAN_POINT('',(-0.230940107675851,0.,0.4));
#9726=CARTESIAN_POINT('Origin',(0.,0.,0.));
#9727=CARTESIAN_POINT('',(-0.2117,0.47,2.59257727379495E-17));
#9728=CARTESIAN_POINT('Origin',(0.,0.47,0.));
#9729=CARTESIAN_POINT('',(-0.2117,0.,2.59257727379495E-17));
#9730=CARTESIAN_POINT('',(-0.2117,0.,2.59257727379495E-17));
#9731=CARTESIAN_POINT('Origin',(0.,0.,0.));
#9732=CARTESIAN_POINT('Origin',(-0.230940107675851,0.,0.4));
#9733=CARTESIAN_POINT('',(0.23094010767585,0.,0.4));
#9734=CARTESIAN_POINT('Origin',(0.461880215351701,0.,0.));
#9735=CARTESIAN_POINT('',(0.461880215351701,0.,0.));
#9736=CARTESIAN_POINT('Origin',(0.23094010767585,0.,0.4));
#9737=CARTESIAN_POINT('Origin',(0.,0.47,0.));
#9738=CARTESIAN_POINT('Origin',(0.,0.,0.));
#9739=CARTESIAN_POINT('',(0.,0.,0.));
#9740=CARTESIAN_POINT('Origin',(0.,-0.6,0.));
#9741=CARTESIAN_POINT('',(1.55884572681199,-0.6,0.));
#9742=CARTESIAN_POINT('',(0.779422863405995,-0.6,1.35));
#9743=CARTESIAN_POINT('',(0.779422863405995,-0.6,1.35));
#9744=CARTESIAN_POINT('',(-0.779422863405996,-0.6,1.35));
#9745=CARTESIAN_POINT('',(-0.779422863405996,-0.6,1.35));
#9746=CARTESIAN_POINT('',(-1.55884572681199,-0.6,-1.90903542970483E-16));
#9747=CARTESIAN_POINT('',(-1.55884572681199,-0.6,-1.90903542970483E-16));
#9748=CARTESIAN_POINT('',(-0.779422863405995,-0.6,-1.35));
#9749=CARTESIAN_POINT('',(-0.779422863405995,-0.6,-1.35));
#9750=CARTESIAN_POINT('',(0.779422863405995,-0.6,-1.35));
#9751=CARTESIAN_POINT('',(0.779422863405995,-0.6,-1.35));
#9752=CARTESIAN_POINT('',(1.55884572681199,-0.6,0.));
#9753=CARTESIAN_POINT('',(-1.065,-0.6,-1.30424884109193E-16));
#9754=CARTESIAN_POINT('Origin',(0.,-0.6,0.));
#9755=CARTESIAN_POINT('Origin',(0.,0.6,0.));
#9756=CARTESIAN_POINT('',(0.779422863405995,0.6,1.35));
#9757=CARTESIAN_POINT('',(1.55884572681199,0.6,0.));
#9758=CARTESIAN_POINT('',(0.779422863405995,0.6,1.35));
#9759=CARTESIAN_POINT('',(0.779422863405995,0.6,-1.35));
#9760=CARTESIAN_POINT('',(1.55884572681199,0.6,0.));
#9761=CARTESIAN_POINT('',(-0.779422863405995,0.6,-1.35));
#9762=CARTESIAN_POINT('',(0.779422863405995,0.6,-1.35));
#9763=CARTESIAN_POINT('',(-1.55884572681199,0.6,-1.90903542970483E-16));
#9764=CARTESIAN_POINT('',(-0.779422863405995,0.6,-1.35));
#9765=CARTESIAN_POINT('',(-0.779422863405996,0.6,1.35));
#9766=CARTESIAN_POINT('',(-1.55884572681199,0.6,-1.90903542970483E-16));
#9767=CARTESIAN_POINT('',(-0.779422863405996,0.6,1.35));
#9768=CARTESIAN_POINT('',(-1.065,0.6,1.30424884109193E-16));
#9769=CARTESIAN_POINT('Origin',(0.,0.6,0.));
#9770=CARTESIAN_POINT('Origin',(-0.779422863405996,0.,1.35));
#9771=CARTESIAN_POINT('',(0.779422863405995,0.,1.35));
#9772=CARTESIAN_POINT('',(-0.779422863405996,0.,1.35));
#9773=CARTESIAN_POINT('Origin',(-1.55884572681199,0.,-1.90903542970483E-16));
#9774=CARTESIAN_POINT('',(-1.55884572681199,0.,-1.90903542970483E-16));
#9775=CARTESIAN_POINT('Origin',(-0.779422863405995,0.,-1.35));
#9776=CARTESIAN_POINT('',(-0.779422863405995,0.,-1.35));
#9777=CARTESIAN_POINT('Origin',(0.779422863405995,0.,-1.35));
#9778=CARTESIAN_POINT('',(0.779422863405995,0.,-1.35));
#9779=CARTESIAN_POINT('Origin',(1.55884572681199,0.,0.));
#9780=CARTESIAN_POINT('',(1.55884572681199,0.,0.));
#9781=CARTESIAN_POINT('Origin',(0.779422863405995,0.,1.35));
#9782=CARTESIAN_POINT('Origin',(0.,0.,0.));
#9783=CARTESIAN_POINT('',(-1.065,2.47,-1.30424884109193E-16));
#9784=CARTESIAN_POINT('',(-1.065,0.,-1.30424884109193E-16));
#9785=CARTESIAN_POINT('Origin',(0.,2.47,0.));
#9786=CARTESIAN_POINT('Origin',(0.985,2.55,0.));
#9787=CARTESIAN_POINT('',(-0.985,2.55,-1.20627709716014E-16));
#9788=CARTESIAN_POINT('Origin',(0.,2.55,0.));
#9789=CARTESIAN_POINT('',(-0.79,2.55,-9.67470971326409E-17));
#9790=CARTESIAN_POINT('Origin',(0.,2.55,0.));
#9791=CARTESIAN_POINT('Origin',(0.,2.51,0.));
#9792=CARTESIAN_POINT('',(-1.025,2.51,-1.25526296912604E-16));
#9793=CARTESIAN_POINT('Origin',(0.,0.,0.));
#9794=CARTESIAN_POINT('',(-1.065,-2.47,-1.30424884109193E-16));
#9795=CARTESIAN_POINT('Origin',(0.,-2.47,0.));
#9796=CARTESIAN_POINT('',(-1.065,0.,-1.30424884109193E-16));
#9797=CARTESIAN_POINT('Origin',(0.,-2.51,0.));
#9798=CARTESIAN_POINT('',(-0.985,-2.55,-1.20627709716014E-16));
#9799=CARTESIAN_POINT('Origin',(0.,-2.55,0.));
#9800=CARTESIAN_POINT('',(-1.025,-2.51,-1.25526296912604E-16));
#9801=CARTESIAN_POINT('Origin',(0.79,-2.55,0.));
#9802=CARTESIAN_POINT('',(-0.79,-2.55,-9.67470971326409E-17));
#9803=CARTESIAN_POINT('Origin',(0.,-2.55,0.));
#9804=CARTESIAN_POINT('Origin',(0.,0.,0.));
#9805=CARTESIAN_POINT('',(-0.79,0.,-9.67470971326409E-17));
#9806=CARTESIAN_POINT('',(0.,0.,0.));
#9807=CARTESIAN_POINT('Origin',(-1.3,-1.,7.5));
#9808=CARTESIAN_POINT('',(-1.525,-1.,8.));
#9809=CARTESIAN_POINT('Origin',(-1.3,-1.,8.));
#9810=CARTESIAN_POINT('',(-1.525,-1.,7.5));
#9811=CARTESIAN_POINT('',(-1.525,-1.,7.5));
#9812=CARTESIAN_POINT('Origin',(-1.3,-1.,7.5));
#9813=CARTESIAN_POINT('Origin',(-1.3,-1.,7.5));
#9814=CARTESIAN_POINT('',(-1.7,-1.,8.));
#9815=CARTESIAN_POINT('Origin',(-1.3,-1.,8.));
#9816=CARTESIAN_POINT('',(-1.7,-1.,7.5));
#9817=CARTESIAN_POINT('',(-1.7,-1.,7.5));
#9818=CARTESIAN_POINT('Origin',(-1.3,-1.,7.5));
#9819=CARTESIAN_POINT('Origin',(-1.3,-1.,8.));
#9820=CARTESIAN_POINT('Origin',(-1.3,-1.,7.5));
#9821=CARTESIAN_POINT('',(0.,0.,0.));
#9822=CARTESIAN_POINT('Origin',(0.3,0.4,0.));
#9823=CARTESIAN_POINT('',(-0.3,0.4,-3.67394039744206E-17));
#9824=CARTESIAN_POINT('Origin',(0.,0.4,0.));
#9825=CARTESIAN_POINT('Origin',(0.,0.375,0.));
#9826=CARTESIAN_POINT('',(-0.35,0.35,-4.28626379701573E-17));
#9827=CARTESIAN_POINT('Origin',(0.,0.35,0.));
#9828=CARTESIAN_POINT('',(-0.325,0.375,-3.9801020972289E-17));
#9829=CARTESIAN_POINT('Origin',(0.,0.19,0.));
#9830=CARTESIAN_POINT('',(-0.35,0.03,-4.28626379701574E-17));
#9831=CARTESIAN_POINT('Origin',(0.,0.03,0.));
#9832=CARTESIAN_POINT('',(-0.35,0.19,-4.28626379701574E-17));
#9833=CARTESIAN_POINT('Origin',(0.,0.0149999999999999,0.));
#9834=CARTESIAN_POINT('',(-0.32,-3.29597460435593E-17,-3.91886975727153E-17));
#9835=CARTESIAN_POINT('Origin',(0.,0.,0.));
#9836=CARTESIAN_POINT('',(-0.335,0.0149999999999999,-4.10256677714363E-17));
#9837=CARTESIAN_POINT('Origin',(0.22,0.,0.));
#9838=CARTESIAN_POINT('',(-0.22,-6.93889390390723E-18,-2.69422295812418E-17));
#9839=CARTESIAN_POINT('Origin',(0.,0.,0.));
#9840=CARTESIAN_POINT('Origin',(0.,-0.02,0.));
#9841=CARTESIAN_POINT('',(-0.1954,-0.0492,2.39295984553393E-17));
#9842=CARTESIAN_POINT('Origin',(0.,-0.0492,0.));
#9843=CARTESIAN_POINT('',(-0.21,-0.02,-2.57175827820944E-17));
#9844=CARTESIAN_POINT('Origin',(0.,-0.8,0.));
#9845=CARTESIAN_POINT('',(-0.1954,-1.5646,2.39295984553393E-17));
#9846=CARTESIAN_POINT('Origin',(0.,-1.5646,0.));
#9847=CARTESIAN_POINT('',(-0.1954,-0.8,-2.39295984553393E-17));
#9848=CARTESIAN_POINT('Origin',(0.,-1.58,0.));
#9849=CARTESIAN_POINT('',(-0.16,-1.6,-1.95943487863577E-17));
#9850=CARTESIAN_POINT('Origin',(0.,-1.6,0.));
#9851=CARTESIAN_POINT('',(-0.18,-1.58,-2.20436423846524E-17));
#9852=CARTESIAN_POINT('Origin',(0.,-1.6,0.));
#9853=CARTESIAN_POINT('Origin',(0.0866025403784439,-0.4,-0.15));
#9854=CARTESIAN_POINT('',(0.173205080756888,-0.4,0.));
#9855=CARTESIAN_POINT('',(0.0866025403784439,-0.4,-0.15));
#9856=CARTESIAN_POINT('',(0.173205080756888,-0.4,0.));
#9857=CARTESIAN_POINT('',(0.0866025403784439,-0.64,-0.15));
#9858=CARTESIAN_POINT('',(0.0866025403784439,-0.4,-0.15));
#9859=CARTESIAN_POINT('',(0.173205080756888,-0.64,0.));
#9860=CARTESIAN_POINT('',(0.173205080756888,-0.64,0.));
#9861=CARTESIAN_POINT('',(0.173205080756888,-0.4,0.));
#9862=CARTESIAN_POINT('Origin',(-0.0866025403784438,-0.4,-0.15));
#9863=CARTESIAN_POINT('',(-0.0866025403784438,-0.4,-0.15));
#9864=CARTESIAN_POINT('',(0.0866025403784439,-0.4,-0.15));
#9865=CARTESIAN_POINT('',(-0.0866025403784438,-0.64,-0.15));
#9866=CARTESIAN_POINT('',(-0.0866025403784438,-0.4,-0.15));
#9867=CARTESIAN_POINT('',(0.0866025403784439,-0.64,-0.15));
#9868=CARTESIAN_POINT('Origin',(-0.173205080756888,-0.4,-2.77555756156289E-17));
#9869=CARTESIAN_POINT('',(-0.173205080756888,-0.4,-2.12115047744981E-17));
#9870=CARTESIAN_POINT('',(-0.0866025403784438,-0.4,-0.15));
#9871=CARTESIAN_POINT('',(-0.173205080756888,-0.64,-2.77555756156289E-17));
#9872=CARTESIAN_POINT('',(-0.173205080756888,-0.4,-2.12115047744981E-17));
#9873=CARTESIAN_POINT('',(-0.0866025403784438,-0.64,-0.15));
#9874=CARTESIAN_POINT('Origin',(-0.0866025403784439,-0.4,0.15));
#9875=CARTESIAN_POINT('',(-0.0866025403784439,-0.4,0.15));
#9876=CARTESIAN_POINT('',(-0.173205080756888,-0.4,-2.12115047744981E-17));
#9877=CARTESIAN_POINT('',(-0.0866025403784439,-0.64,0.15));
#9878=CARTESIAN_POINT('',(-0.0866025403784439,-0.4,0.15));
#9879=CARTESIAN_POINT('',(-0.173205080756888,-0.64,-2.12115047744981E-17));
#9880=CARTESIAN_POINT('Origin',(0.0866025403784439,-0.4,0.15));
#9881=CARTESIAN_POINT('',(0.0866025403784439,-0.4,0.15));
#9882=CARTESIAN_POINT('',(-0.0866025403784439,-0.4,0.15));
#9883=CARTESIAN_POINT('',(0.0866025403784439,-0.64,0.15));
#9884=CARTESIAN_POINT('',(0.0866025403784439,-0.4,0.15));
#9885=CARTESIAN_POINT('',(-0.0866025403784439,-0.64,0.15));
#9886=CARTESIAN_POINT('Origin',(0.173205080756888,-0.4,0.));
#9887=CARTESIAN_POINT('',(0.0866025403784439,-0.4,0.15));
#9888=CARTESIAN_POINT('',(0.0866025403784439,-0.64,0.15));
#9889=CARTESIAN_POINT('Origin',(0.,-0.4,-2.77555756156289E-17));
#9890=CARTESIAN_POINT('Origin',(0.,-0.64,-2.77555756156289E-17));
#9891=CARTESIAN_POINT('',(0.,0.,0.));
#9892=CARTESIAN_POINT('Origin',(3.,1.1,8.2));
#9893=CARTESIAN_POINT('',(2.7,1.1,9.4));
#9894=CARTESIAN_POINT('Origin',(3.,1.1,9.4));
#9895=CARTESIAN_POINT('',(2.7,1.1,8.2));
#9896=CARTESIAN_POINT('',(2.7,1.1,8.2));
#9897=CARTESIAN_POINT('Origin',(3.,1.1,8.2));
#9898=CARTESIAN_POINT('Origin',(3.,1.1,9.4));
#9899=CARTESIAN_POINT('Origin',(3.,1.1,8.2));
#9900=CARTESIAN_POINT('',(0.,0.,0.));
#9901=CARTESIAN_POINT('Origin',(0.,-0.1,0.));
#9902=CARTESIAN_POINT('',(0.227088088635226,0.227088088635225,0.400038748123229));
#9903=CARTESIAN_POINT('',(0.227088088635226,0.227088088635225,-0.400038748123229));
#9904=CARTESIAN_POINT('Origin',(0.,0.,0.));
#9905=CARTESIAN_POINT('',(-0.46,0.227088088635226,5.63337527607782E-17));
#9906=CARTESIAN_POINT('Origin',(0.,0.227088088635226,0.));
#9907=CARTESIAN_POINT('',(-0.46,1.1,-5.63337527607782E-17));
#9908=CARTESIAN_POINT('',(-0.46,-0.1,5.63337527607782E-17));
#9909=CARTESIAN_POINT('Origin',(0.,1.1,0.));
#9910=CARTESIAN_POINT('Origin',(0.,0.227088088635226,0.));
#9911=CARTESIAN_POINT('Origin',(0.,0.,0.));
#9912=CARTESIAN_POINT('',(-3.14121903981296E-17,-3.84688384252766E-33,-0.513));
#9913=CARTESIAN_POINT('',(-3.14121903981296E-17,-3.84688384252766E-33,0.513));
#9914=CARTESIAN_POINT('Origin',(0.,0.,0.));
#9915=CARTESIAN_POINT('',(0.227088088635226,-5.63337527607782E-17,0.46));
#9916=CARTESIAN_POINT('Origin',(0.227088088635226,0.,0.));
#9917=CARTESIAN_POINT('Origin',(0.227088088635226,0.,0.));
#9918=CARTESIAN_POINT('Origin',(-0.1,0.,0.));
#9919=CARTESIAN_POINT('',(1.1,5.63337527607782E-17,0.46));
#9920=CARTESIAN_POINT('',(-0.1,-5.63337527607782E-17,0.46));
#9921=CARTESIAN_POINT('Origin',(1.1,0.,0.));
#9922=CARTESIAN_POINT('Origin',(0.,1.1,0.));
#9923=CARTESIAN_POINT('',(-0.57,1.1,-6.98048675513991E-17));
#9924=CARTESIAN_POINT('Origin',(0.,1.1,0.));
#9925=CARTESIAN_POINT('Origin',(0.,1.65,0.));
#9926=CARTESIAN_POINT('',(-0.57,2.1,-6.98048675513991E-17));
#9927=CARTESIAN_POINT('Origin',(0.,2.1,0.));
#9928=CARTESIAN_POINT('',(-0.57,1.65,-6.98048675513991E-17));
#9929=CARTESIAN_POINT('Origin',(1.65,0.,0.));
#9930=CARTESIAN_POINT('',(1.1,-0.57,-6.98048675513991E-17));
#9931=CARTESIAN_POINT('Origin',(1.1,0.,0.));
#9932=CARTESIAN_POINT('',(2.1,-0.57,6.98048675513991E-17));
#9933=CARTESIAN_POINT('',(1.65,-0.57,-6.98048675513991E-17));
#9934=CARTESIAN_POINT('Origin',(2.1,0.,0.));
#9935=CARTESIAN_POINT('Origin',(1.1,0.57,0.));
#9936=CARTESIAN_POINT('Origin',(0.,0.,0.));
#9937=CARTESIAN_POINT('',(0.,0.,0.825));
#9938=CARTESIAN_POINT('',(-0.825,0.,-1.01033360929657E-16));
#9939=CARTESIAN_POINT('Origin',(0.,0.,0.));
#9940=CARTESIAN_POINT('',(0.,0.,-0.825));
#9941=CARTESIAN_POINT('Origin',(0.,0.,0.));
#9942=CARTESIAN_POINT('',(0.,-0.825,-1.01033360929657E-16));
#9943=CARTESIAN_POINT('Origin',(0.,0.,0.));
#9944=CARTESIAN_POINT('Origin',(0.,0.,0.));
#9945=CARTESIAN_POINT('Origin',(0.,0.7,0.));
#9946=CARTESIAN_POINT('Origin',(0.,0.,0.));
#9947=CARTESIAN_POINT('',(-0.825,1.4,-1.01033360929657E-16));
#9948=CARTESIAN_POINT('',(-0.825,0.7,-1.01033360929657E-16));
#9949=CARTESIAN_POINT('Origin',(0.,1.4,0.));
#9950=CARTESIAN_POINT('Origin',(1.,2.1,0.));
#9951=CARTESIAN_POINT('',(-1.,2.1,-1.22464679914735E-16));
#9952=CARTESIAN_POINT('Origin',(0.,2.1,0.));
#9953=CARTESIAN_POINT('Origin',(0.,1.75,0.));
#9954=CARTESIAN_POINT('',(-1.,1.4,-1.22464679914735E-16));
#9955=CARTESIAN_POINT('Origin',(0.,1.4,0.));
#9956=CARTESIAN_POINT('',(-1.,1.75,-1.22464679914735E-16));
#9957=CARTESIAN_POINT('Origin',(0.825,1.4,0.));
#9958=CARTESIAN_POINT('Origin',(1.4,1.,0.));
#9959=CARTESIAN_POINT('',(1.4,-1.,-1.22464679914735E-16));
#9960=CARTESIAN_POINT('Origin',(1.4,0.,0.));
#9961=CARTESIAN_POINT('',(1.4,-0.825,-1.01033360929657E-16));
#9962=CARTESIAN_POINT('Origin',(1.4,0.,0.));
#9963=CARTESIAN_POINT('Origin',(1.75,0.,0.));
#9964=CARTESIAN_POINT('',(2.1,-1.,-1.22464679914735E-16));
#9965=CARTESIAN_POINT('Origin',(2.1,0.,0.));
#9966=CARTESIAN_POINT('',(1.75,-1.,-1.22464679914735E-16));
#9967=CARTESIAN_POINT('Origin',(2.1,0.,0.));
#9968=CARTESIAN_POINT('Origin',(0.7,0.,0.));
#9969=CARTESIAN_POINT('',(0.7,-0.825,-1.01033360929657E-16));
#9970=CARTESIAN_POINT('',(0.,0.,0.));
#9971=CARTESIAN_POINT('Origin',(0.,-0.4,0.));
#9972=CARTESIAN_POINT('',(1.01036297108185,-0.4,0.));
#9973=CARTESIAN_POINT('',(0.505181485540923,-0.4,0.875));
#9974=CARTESIAN_POINT('',(0.505181485540923,-0.4,0.875));
#9975=CARTESIAN_POINT('',(-0.505181485540923,-0.4,0.875));
#9976=CARTESIAN_POINT('',(-0.505181485540923,-0.4,0.875));
#9977=CARTESIAN_POINT('',(-1.01036297108185,-0.4,-1.23733777851239E-16));
#9978=CARTESIAN_POINT('',(-1.01036297108185,-0.4,-1.23733777851239E-16));
#9979=CARTESIAN_POINT('',(-0.505181485540922,-0.4,-0.875));
#9980=CARTESIAN_POINT('',(-0.505181485540922,-0.4,-0.875));
#9981=CARTESIAN_POINT('',(0.505181485540923,-0.4,-0.875));
#9982=CARTESIAN_POINT('',(0.505181485540923,-0.4,-0.875));
#9983=CARTESIAN_POINT('',(1.01036297108185,-0.4,0.));
#9984=CARTESIAN_POINT('',(-0.685,-0.4,-8.38883057415937E-17));
#9985=CARTESIAN_POINT('Origin',(0.,-0.4,0.));
#9986=CARTESIAN_POINT('Origin',(0.,0.4,0.));
#9987=CARTESIAN_POINT('',(0.505181485540923,0.4,0.875));
#9988=CARTESIAN_POINT('',(1.01036297108185,0.4,0.));
#9989=CARTESIAN_POINT('',(0.505181485540923,0.4,0.875));
#9990=CARTESIAN_POINT('',(0.505181485540923,0.4,-0.875));
#9991=CARTESIAN_POINT('',(1.01036297108185,0.4,0.));
#9992=CARTESIAN_POINT('',(-0.505181485540922,0.4,-0.875));
#9993=CARTESIAN_POINT('',(0.505181485540923,0.4,-0.875));
#9994=CARTESIAN_POINT('',(-1.01036297108185,0.4,-1.23733777851239E-16));
#9995=CARTESIAN_POINT('',(-0.505181485540922,0.4,-0.875));
#9996=CARTESIAN_POINT('',(-0.505181485540923,0.4,0.875));
#9997=CARTESIAN_POINT('',(-1.01036297108185,0.4,-1.23733777851239E-16));
#9998=CARTESIAN_POINT('',(-0.505181485540923,0.4,0.875));
#9999=CARTESIAN_POINT('',(-0.685,0.4,8.38883057415937E-17));
#10000=CARTESIAN_POINT('Origin',(0.,0.4,0.));
#10001=CARTESIAN_POINT('Origin',(-0.505181485540923,0.,0.875));
#10002=CARTESIAN_POINT('',(0.505181485540923,0.,0.875));
#10003=CARTESIAN_POINT('',(-0.505181485540923,0.,0.875));
#10004=CARTESIAN_POINT('Origin',(-1.01036297108185,0.,-1.23733777851239E-16));
#10005=CARTESIAN_POINT('',(-1.01036297108185,0.,-1.23733777851239E-16));
#10006=CARTESIAN_POINT('Origin',(-0.505181485540922,0.,-0.875));
#10007=CARTESIAN_POINT('',(-0.505181485540922,0.,-0.875));
#10008=CARTESIAN_POINT('Origin',(0.505181485540923,0.,-0.875));
#10009=CARTESIAN_POINT('',(0.505181485540923,0.,-0.875));
#10010=CARTESIAN_POINT('Origin',(1.01036297108185,0.,0.));
#10011=CARTESIAN_POINT('',(1.01036297108185,0.,0.));
#10012=CARTESIAN_POINT('Origin',(0.505181485540923,0.,0.875));
#10013=CARTESIAN_POINT('Origin',(0.,0.,0.));
#10014=CARTESIAN_POINT('',(-0.685,1.82,-8.38883057415937E-17));
#10015=CARTESIAN_POINT('',(-0.685,0.,-8.38883057415937E-17));
#10016=CARTESIAN_POINT('Origin',(0.,1.82,0.));
#10017=CARTESIAN_POINT('Origin',(0.605,1.9,0.));
#10018=CARTESIAN_POINT('',(-0.605,1.9,-7.40911313484149E-17));
#10019=CARTESIAN_POINT('Origin',(0.,1.9,0.));
#10020=CARTESIAN_POINT('',(-0.46,1.9,-5.63337527607782E-17));
#10021=CARTESIAN_POINT('Origin',(0.,1.9,0.));
#10022=CARTESIAN_POINT('Origin',(0.,1.86,0.));
#10023=CARTESIAN_POINT('',(-0.645,1.86,-7.89897185450043E-17));
#10024=CARTESIAN_POINT('Origin',(0.,0.,0.));
#10025=CARTESIAN_POINT('',(-0.685,-1.82,-8.38883057415937E-17));
#10026=CARTESIAN_POINT('Origin',(0.,-1.82,0.));
#10027=CARTESIAN_POINT('',(-0.685,0.,-8.38883057415937E-17));
#10028=CARTESIAN_POINT('Origin',(0.,-1.86,0.));
#10029=CARTESIAN_POINT('',(-0.605,-1.9,-7.40911313484149E-17));
#10030=CARTESIAN_POINT('Origin',(0.,-1.9,0.));
#10031=CARTESIAN_POINT('',(-0.645,-1.86,-7.89897185450043E-17));
#10032=CARTESIAN_POINT('Origin',(0.46,-1.9,0.));
#10033=CARTESIAN_POINT('',(-0.46,-1.9,-5.63337527607782E-17));
#10034=CARTESIAN_POINT('Origin',(0.,-1.9,0.));
#10035=CARTESIAN_POINT('Origin',(0.,0.,0.));
#10036=CARTESIAN_POINT('',(-0.46,0.,-5.63337527607782E-17));
#10037=CARTESIAN_POINT('',(0.,0.,0.));
#10038=CARTESIAN_POINT('Origin',(0.,-1.445,0.));
#10039=CARTESIAN_POINT('',(-0.2942,-2.9458,3.60291088309151E-17));
#10040=CARTESIAN_POINT('Origin',(0.,-2.9458,0.));
#10041=CARTESIAN_POINT('',(-0.2942,0.,-3.60291088309151E-17));
#10042=CARTESIAN_POINT('',(-0.2942,-1.445,-3.60291088309151E-17));
#10043=CARTESIAN_POINT('Origin',(0.,0.,0.));
#10044=CARTESIAN_POINT('Origin',(0.,-2.97,0.));
#10045=CARTESIAN_POINT('',(-0.24,-3.,-2.93915231795365E-17));
#10046=CARTESIAN_POINT('Origin',(0.,-3.,0.));
#10047=CARTESIAN_POINT('',(-0.27,-2.97,-3.30654635769785E-17));
#10048=CARTESIAN_POINT('Origin',(0.,-3.,0.));
#10049=CARTESIAN_POINT('Origin',(0.,0.341586508806388,0.));
#10050=CARTESIAN_POINT('',(-0.475,0.4,-5.81707229594993E-17));
#10051=CARTESIAN_POINT('Origin',(0.,0.4,0.));
#10052=CARTESIAN_POINT('',(-0.577350269189626,0.340908044531739,-7.07050159149938E-17));
#10053=CARTESIAN_POINT('',(-0.576175134594813,0.341586508806388,-7.05611034329833E-17));
#10054=CARTESIAN_POINT('',(-0.288675134594813,0.340908044531739,0.5));
#10055=CARTESIAN_POINT('Ctrl Pts',(-0.288675134594813,0.340908044531739,
0.5));
#10056=CARTESIAN_POINT('Ctrl Pts',(-0.433012701893303,0.424241377863696,
0.249999999998124));
#10057=CARTESIAN_POINT('Ctrl Pts',(-0.577350269189626,0.340908044531739,
-7.07050159149938E-17));
#10058=CARTESIAN_POINT('',(0.288675134594813,0.340908044531739,0.5));
#10059=CARTESIAN_POINT('Ctrl Pts',(0.288675134594813,0.340908044531739,
0.5));
#10060=CARTESIAN_POINT('Ctrl Pts',(-2.16648921025353E-12,0.424241377863696,
0.5));
#10061=CARTESIAN_POINT('Ctrl Pts',(-0.288675134594813,0.340908044531739,
0.5));
#10062=CARTESIAN_POINT('',(0.577350269189626,0.340908044531739,0.));
#10063=CARTESIAN_POINT('Ctrl Pts',(0.577350269189626,0.340908044531739,
0.));
#10064=CARTESIAN_POINT('Ctrl Pts',(0.433012701891136,0.424241377863697,
0.250000000001876));
#10065=CARTESIAN_POINT('Ctrl Pts',(0.288675134594813,0.340908044531739,
0.5));
#10066=CARTESIAN_POINT('',(0.288675134594813,0.340908044531739,-0.5));
#10067=CARTESIAN_POINT('Ctrl Pts',(0.288675134594813,0.340908044531739,
-0.5));
#10068=CARTESIAN_POINT('Ctrl Pts',(0.433012701893303,0.424241377863696,
-0.249999999998124));
#10069=CARTESIAN_POINT('Ctrl Pts',(0.577350269189626,0.340908044531739,
0.));
#10070=CARTESIAN_POINT('',(-0.288675134594813,0.340908044531739,-0.5));
#10071=CARTESIAN_POINT('Ctrl Pts',(-0.288675134594813,0.340908044531739,
-0.5));
#10072=CARTESIAN_POINT('Ctrl Pts',(2.16660023255599E-12,0.424241377863696,
-0.5));
#10073=CARTESIAN_POINT('Ctrl Pts',(0.288675134594813,0.340908044531739,
-0.5));
#10074=CARTESIAN_POINT('Ctrl Pts',(-0.577350269189626,0.340908044531739,
-7.07050159149938E-17));
#10075=CARTESIAN_POINT('Ctrl Pts',(-0.433012701891136,0.424241377863697,
-0.250000000001876));
#10076=CARTESIAN_POINT('Ctrl Pts',(-0.288675134594813,0.340908044531739,
-0.5));
#10077=CARTESIAN_POINT('Origin',(0.288675134594813,0.,-0.5));
#10078=CARTESIAN_POINT('',(0.288675134594813,0.,-0.5));
#10079=CARTESIAN_POINT('',(0.288675134594813,0.,-0.5));
#10080=CARTESIAN_POINT('',(-0.288675134594813,0.,-0.5));
#10081=CARTESIAN_POINT('',(0.288675134594813,0.,-0.5));
#10082=CARTESIAN_POINT('',(-0.288675134594813,0.,-0.5));
#10083=CARTESIAN_POINT('Origin',(0.577350269189626,0.,0.));
#10084=CARTESIAN_POINT('',(0.577350269189626,0.,0.));
#10085=CARTESIAN_POINT('',(0.577350269189626,0.,0.));
#10086=CARTESIAN_POINT('',(0.577350269189626,0.,0.));
#10087=CARTESIAN_POINT('Origin',(0.288675134594813,0.,0.5));
#10088=CARTESIAN_POINT('',(0.288675134594813,0.,0.5));
#10089=CARTESIAN_POINT('',(0.288675134594813,0.,0.5));
#10090=CARTESIAN_POINT('',(0.288675134594813,0.,0.5));
#10091=CARTESIAN_POINT('Origin',(-0.288675134594813,0.,0.5));
#10092=CARTESIAN_POINT('',(-0.288675134594813,0.,0.5));
#10093=CARTESIAN_POINT('',(-0.288675134594813,0.,0.5));
#10094=CARTESIAN_POINT('',(-0.288675134594813,0.,0.5));
#10095=CARTESIAN_POINT('Origin',(-0.577350269189626,0.,-7.07050159149938E-17));
#10096=CARTESIAN_POINT('',(-0.577350269189626,0.,-7.07050159149938E-17));
#10097=CARTESIAN_POINT('',(-0.577350269189626,0.,-7.07050159149938E-17));
#10098=CARTESIAN_POINT('',(-0.577350269189626,0.,-7.07050159149938E-17));
#10099=CARTESIAN_POINT('Origin',(-0.288675134594813,0.,-0.5));
#10100=CARTESIAN_POINT('',(-0.288675134594813,0.,-0.5));
#10101=CARTESIAN_POINT('Origin',(0.,0.4,0.));
#10102=CARTESIAN_POINT('Origin',(0.,0.,0.));
#10103=CARTESIAN_POINT('',(0.,0.,0.));
#10104=CARTESIAN_POINT('',(0.,0.,0.));
#10105=CARTESIAN_POINT('',(0.,0.,0.));
#10106=CARTESIAN_POINT('',(0.,0.,0.));
#10107=CARTESIAN_POINT('',(0.,0.,0.));
#10108=CARTESIAN_POINT('',(0.,0.,0.));
#10109=CARTESIAN_POINT('',(0.,0.,0.));
#10110=CARTESIAN_POINT('',(0.,0.,0.));
#10111=CARTESIAN_POINT('',(0.,0.,0.));
#10112=CARTESIAN_POINT('',(0.,0.,0.));
#10113=CARTESIAN_POINT('',(0.,0.,0.));
#10114=CARTESIAN_POINT('',(0.,0.,0.));
#10115=CARTESIAN_POINT('',(0.,0.,0.));
#10116=CARTESIAN_POINT('',(0.,0.,0.));
#10117=CARTESIAN_POINT('',(-1.9,-3.,3.1));
#10118=CARTESIAN_POINT('',(-1.9,-3.1,3.1));
#10119=CARTESIAN_POINT('',(-1.9,3.,3.1));
#10120=CARTESIAN_POINT('',(-1.9,3.1,3.1));
#10121=CARTESIAN_POINT('',(-1.9,-3.,6.9));
#10122=CARTESIAN_POINT('',(-1.9,-3.1,6.9));
#10123=CARTESIAN_POINT('',(-1.9,3.,6.9));
#10124=CARTESIAN_POINT('',(-1.9,3.1,6.9));
#10125=CARTESIAN_POINT('',(1.9,-3.,3.1));
#10126=CARTESIAN_POINT('',(1.9,-3.1,3.1));
#10127=CARTESIAN_POINT('',(1.9,3.,3.1));
#10128=CARTESIAN_POINT('',(1.9,3.1,3.1));
#10129=CARTESIAN_POINT('',(1.9,-3.,6.9));
#10130=CARTESIAN_POINT('',(1.9,-3.1,6.9));
#10131=CARTESIAN_POINT('',(1.9,3.,6.9));
#10132=CARTESIAN_POINT('',(1.9,3.1,6.9));
#10133=CARTESIAN_POINT('',(0.,-4.35,5.));
#10134=CARTESIAN_POINT('',(0.,4.35,5.));
#10135=CARTESIAN_POINT('',(0.,0.,0.));
#10136=CARTESIAN_POINT('',(-1.3,-1.,8.5));
#10137=CARTESIAN_POINT('',(0.,2.,0.));
#10138=CARTESIAN_POINT('',(-1.3,1.,8.5));
#10139=CARTESIAN_POINT('',(2.6,0.,0.));
#10140=CARTESIAN_POINT('',(1.3,-1.,8.5));
#10141=CARTESIAN_POINT('',(2.6,2.,0.));
#10142=CARTESIAN_POINT('',(1.3,1.,8.5));
#10143=CARTESIAN_POINT('',(0.,0.,0.));
#10144=CARTESIAN_POINT('',(-4.1,-4.1,0.));
#10145=CARTESIAN_POINT('',(0.,-9.4,5.));
#10146=CARTESIAN_POINT('',(0.,-12.4,5.));
#10147=CARTESIAN_POINT('',(-3.,-12.4,5.));
#10148=CARTESIAN_POINT('',(2.2,-7.,7.));
#10149=CARTESIAN_POINT('',(2.2,7.,7.));
#10150=CARTESIAN_POINT('',(0.,0.,0.));
#10151=CARTESIAN_POINT('',(0.,0.,0.));
#10152=CARTESIAN_POINT('Origin',(-0.205,-0.205,6.));
#10153=CARTESIAN_POINT('',(0.205,-0.205,6.47171668469172));
#10154=CARTESIAN_POINT('',(-0.205,-0.205,6.47171668469172));
#10155=CARTESIAN_POINT('Origin',(0.,-0.205,5.));
#10156=CARTESIAN_POINT('',(0.205,-0.205,6.));
#10157=CARTESIAN_POINT('',(0.205,-0.205,6.));
#10158=CARTESIAN_POINT('',(-0.205,-0.205,6.));
#10159=CARTESIAN_POINT('',(-0.205,-0.205,6.));
#10160=CARTESIAN_POINT('',(-0.205,-0.205,6.));
#10161=CARTESIAN_POINT('Origin',(-0.205,0.205,6.));
#10162=CARTESIAN_POINT('',(-0.205,-2.51052593825207E-17,6.48592563743951));
#10163=CARTESIAN_POINT('Origin',(-0.205,0.,5.));
#10164=CARTESIAN_POINT('',(-0.205,0.205,6.));
#10165=CARTESIAN_POINT('',(-0.205,0.205,6.));
#10166=CARTESIAN_POINT('',(-0.205,0.205,6.47171668469172));
#10167=CARTESIAN_POINT('',(-0.205,0.205,6.));
#10168=CARTESIAN_POINT('Origin',(-0.205,0.,5.));
#10169=CARTESIAN_POINT('Origin',(0.205,0.205,6.));
#10170=CARTESIAN_POINT('',(0.205,0.205,6.47171668469172));
#10171=CARTESIAN_POINT('Origin',(0.,0.205,5.));
#10172=CARTESIAN_POINT('',(0.205,0.205,6.));
#10173=CARTESIAN_POINT('',(0.205,0.205,6.));
#10174=CARTESIAN_POINT('',(0.205,0.205,6.));
#10175=CARTESIAN_POINT('Origin',(0.205,-0.205,6.));
#10176=CARTESIAN_POINT('Origin',(0.205,0.,5.));
#10177=CARTESIAN_POINT('',(0.205,-0.205,6.));
#10178=CARTESIAN_POINT('Origin',(0.,0.,6.));
#10179=CARTESIAN_POINT('Origin',(0.,-1.6,5.));
#10180=CARTESIAN_POINT('',(-0.75,-1.29903810567666,5.));
#10181=CARTESIAN_POINT('Origin',(0.,-1.29903810567666,5.));
#10182=CARTESIAN_POINT('',(-0.75,1.29903810567666,5.));
#10183=CARTESIAN_POINT('',(-0.75,-1.6,5.));
#10184=CARTESIAN_POINT('Origin',(0.,1.29903810567666,5.));
#10185=CARTESIAN_POINT('Origin',(0.,0.,5.));
#10186=CARTESIAN_POINT('',(-9.18485099360515E-17,-1.12481983699639E-32,
3.5));
#10187=CARTESIAN_POINT('Origin',(0.,0.,5.));
#10188=CARTESIAN_POINT('',(0.,0.,0.));
#10189=CARTESIAN_POINT('Origin',(0.,0.,8.5));
#10190=CARTESIAN_POINT('',(-0.165,-2.02066721859313E-17,8.5));
#10191=CARTESIAN_POINT('Origin',(0.,0.,8.5));
#10192=CARTESIAN_POINT('',(-0.165,2.02066721859313E-17,9.4));
#10193=CARTESIAN_POINT('',(-0.165,-2.02066721859313E-17,8.5));
#10194=CARTESIAN_POINT('Origin',(0.,0.,9.4));
#10195=CARTESIAN_POINT('Origin',(0.,0.,8.5));
#10196=CARTESIAN_POINT('Origin',(0.,0.,8.7));
#10197=CARTESIAN_POINT('',(-0.264575131106459,0.3,8.7));
#10198=CARTESIAN_POINT('',(-0.3,0.264575131106459,8.7));
#10199=CARTESIAN_POINT('Origin',(0.,0.,8.7));
#10200=CARTESIAN_POINT('',(-0.3,0.3,8.7));
#10201=CARTESIAN_POINT('',(-0.3,0.3,8.7));
#10202=CARTESIAN_POINT('',(0.3,0.3,8.7));
#10203=CARTESIAN_POINT('Origin',(0.,0.,8.7));
#10204=CARTESIAN_POINT('',(-0.3,-0.264575131106459,8.7));
#10205=CARTESIAN_POINT('',(-0.264575131106459,-0.3,8.7));
#10206=CARTESIAN_POINT('Origin',(0.,0.,8.7));
#10207=CARTESIAN_POINT('',(-0.3,-0.3,8.7));
#10208=CARTESIAN_POINT('',(-0.3,-0.3,8.7));
#10209=CARTESIAN_POINT('',(-0.3,0.3,8.7));
#10210=CARTESIAN_POINT('Origin',(0.,0.,8.7));
#10211=CARTESIAN_POINT('',(0.264575131106459,-0.3,8.7));
#10212=CARTESIAN_POINT('',(0.3,-0.264575131106459,8.7));
#10213=CARTESIAN_POINT('Origin',(0.,0.,8.7));
#10214=CARTESIAN_POINT('',(0.3,-0.3,8.7));
#10215=CARTESIAN_POINT('',(0.3,-0.3,8.7));
#10216=CARTESIAN_POINT('',(-0.3,-0.3,8.7));
#10217=CARTESIAN_POINT('Origin',(0.,0.,8.7));
#10218=CARTESIAN_POINT('',(0.3,0.264575131106459,8.7));
#10219=CARTESIAN_POINT('',(0.264575131106459,0.3,8.7));
#10220=CARTESIAN_POINT('Origin',(0.,0.,8.7));
#10221=CARTESIAN_POINT('',(0.3,0.3,8.7));
#10222=CARTESIAN_POINT('',(0.3,0.3,8.7));
#10223=CARTESIAN_POINT('',(0.3,-0.3,8.7));
#10224=CARTESIAN_POINT('Origin',(0.3,0.3,8.7));
#10225=CARTESIAN_POINT('',(0.15,0.3,8.7));
#10226=CARTESIAN_POINT('',(-0.3,0.3,9.4));
#10227=CARTESIAN_POINT('',(-0.3,0.3,8.7));
#10228=CARTESIAN_POINT('',(0.3,0.3,9.4));
#10229=CARTESIAN_POINT('',(0.3,0.3,9.4));
#10230=CARTESIAN_POINT('',(0.3,0.3,8.7));
#10231=CARTESIAN_POINT('Origin',(0.3,-0.3,8.7));
#10232=CARTESIAN_POINT('',(0.3,-0.15,8.7));
#10233=CARTESIAN_POINT('',(0.3,-0.3,9.4));
#10234=CARTESIAN_POINT('',(0.3,-0.3,9.4));
#10235=CARTESIAN_POINT('',(0.3,-0.3,8.7));
#10236=CARTESIAN_POINT('Origin',(-0.3,-0.3,8.7));
#10237=CARTESIAN_POINT('',(-0.15,-0.3,8.7));
#10238=CARTESIAN_POINT('',(-0.3,-0.3,9.4));
#10239=CARTESIAN_POINT('',(-0.3,-0.3,9.4));
#10240=CARTESIAN_POINT('',(-0.3,-0.3,8.7));
#10241=CARTESIAN_POINT('Origin',(-0.3,0.3,8.7));
#10242=CARTESIAN_POINT('',(-0.3,0.15,8.7));
#10243=CARTESIAN_POINT('',(-0.3,0.3,9.4));
#10244=CARTESIAN_POINT('Origin',(0.,0.,9.4));
#10245=CARTESIAN_POINT('Origin',(0.,0.,8.7));
#10246=CARTESIAN_POINT('Origin',(0.,0.,8.7));
#10247=CARTESIAN_POINT('Origin',(0.,0.,8.7));
#10248=CARTESIAN_POINT('',(-0.4,-4.89858719658941E-17,8.7));
#10249=CARTESIAN_POINT('Origin',(0.,0.,8.7));
#10250=CARTESIAN_POINT('Origin',(0.,0.,8.7));
#10251=CARTESIAN_POINT('Origin',(0.,0.,8.7));
#10252=CARTESIAN_POINT('Origin',(0.,0.,8.7));
#10253=CARTESIAN_POINT('Origin',(0.,0.,8.7));
#10254=CARTESIAN_POINT('Origin',(0.,0.,8.7));
#10255=CARTESIAN_POINT('Origin',(0.2,0.2,6.));
#10256=CARTESIAN_POINT('',(0.2,0.2,6.));
#10257=CARTESIAN_POINT('',(-0.2,0.2,6.));
#10258=CARTESIAN_POINT('',(0.2,0.2,6.));
#10259=CARTESIAN_POINT('',(-0.2,0.2,6.5));
#10260=CARTESIAN_POINT('',(-0.2,0.2,6.));
#10261=CARTESIAN_POINT('',(0.2,0.2,6.5));
#10262=CARTESIAN_POINT('',(0.1,0.2,6.5));
#10263=CARTESIAN_POINT('',(0.2,0.2,6.));
#10264=CARTESIAN_POINT('Origin',(0.2,-0.2,6.));
#10265=CARTESIAN_POINT('',(0.2,-0.2,6.));
#10266=CARTESIAN_POINT('',(0.2,-0.2,6.));
#10267=CARTESIAN_POINT('',(0.2,-0.2,6.5));
#10268=CARTESIAN_POINT('',(0.2,-0.1,6.5));
#10269=CARTESIAN_POINT('',(0.2,-0.2,6.));
#10270=CARTESIAN_POINT('Origin',(-0.2,-0.2,6.));
#10271=CARTESIAN_POINT('',(-0.2,-0.2,6.));
#10272=CARTESIAN_POINT('',(-0.2,-0.2,6.));
#10273=CARTESIAN_POINT('',(-0.2,-0.2,6.5));
#10274=CARTESIAN_POINT('',(-0.1,-0.2,6.5));
#10275=CARTESIAN_POINT('',(-0.2,-0.2,6.));
#10276=CARTESIAN_POINT('Origin',(-0.2,0.2,6.));
#10277=CARTESIAN_POINT('',(-0.2,0.2,6.));
#10278=CARTESIAN_POINT('',(-0.2,0.1,6.5));
#10279=CARTESIAN_POINT('Origin',(0.,0.,6.));
#10280=CARTESIAN_POINT('Origin',(0.,0.,6.5));
#10281=CARTESIAN_POINT('',(-0.4,-4.89858719658941E-17,6.5));
#10282=CARTESIAN_POINT('',(-0.4,-4.89858719658941E-17,6.5));
#10283=CARTESIAN_POINT('Origin',(0.,0.,6.5));
#10284=CARTESIAN_POINT('Origin',(0.,0.,6.5));
#10285=CARTESIAN_POINT('',(0.,0.,0.));
#10286=CARTESIAN_POINT('Origin',(-0.305,-0.305,8.9));
#10287=CARTESIAN_POINT('',(0.305,-0.305,9.4));
#10288=CARTESIAN_POINT('',(-0.305,-0.305,9.4));
#10289=CARTESIAN_POINT('',(1.6475,-0.305,9.4));
#10290=CARTESIAN_POINT('',(0.305,-0.305,9.));
#10291=CARTESIAN_POINT('',(0.305,-0.305,8.9));
#10292=CARTESIAN_POINT('',(-0.305,-0.305,9.));
#10293=CARTESIAN_POINT('',(1.6475,-0.305,9.));
#10294=CARTESIAN_POINT('',(-0.305,-0.305,8.9));
#10295=CARTESIAN_POINT('Origin',(-0.305,0.305,8.9));
#10296=CARTESIAN_POINT('',(-0.305,0.305,9.4));
#10297=CARTESIAN_POINT('',(-0.305,0.1525,9.4));
#10298=CARTESIAN_POINT('',(-0.305,0.305,9.));
#10299=CARTESIAN_POINT('',(-0.305,0.1525,9.));
#10300=CARTESIAN_POINT('',(-0.305,0.305,8.9));
#10301=CARTESIAN_POINT('Origin',(0.305,0.305,8.9));
#10302=CARTESIAN_POINT('',(0.305,0.305,9.4));
#10303=CARTESIAN_POINT('',(1.9525,0.305,9.4));
#10304=CARTESIAN_POINT('',(0.305,0.305,9.));
#10305=CARTESIAN_POINT('',(1.9525,0.305,9.));
#10306=CARTESIAN_POINT('',(0.305,0.305,8.9));
#10307=CARTESIAN_POINT('Origin',(0.305,-0.305,8.9));
#10308=CARTESIAN_POINT('',(0.305,-0.1525,9.4));
#10309=CARTESIAN_POINT('',(0.305,-0.1525,9.));
#10310=CARTESIAN_POINT('Origin',(8.,0.8,9.));
#10311=CARTESIAN_POINT('',(8.,0.8,9.));
#10312=CARTESIAN_POINT('',(-0.8,0.8,9.));
#10313=CARTESIAN_POINT('',(8.,0.8,9.));
#10314=CARTESIAN_POINT('',(-0.8,0.8,9.4));
#10315=CARTESIAN_POINT('',(-0.8,0.8,9.));
#10316=CARTESIAN_POINT('',(8.,0.8,9.4));
#10317=CARTESIAN_POINT('',(8.,0.8,9.4));
#10318=CARTESIAN_POINT('',(8.,0.8,9.));
#10319=CARTESIAN_POINT('Origin',(8.,-0.8,9.));
#10320=CARTESIAN_POINT('',(8.,-0.8,9.));
#10321=CARTESIAN_POINT('',(8.,-0.8,9.));
#10322=CARTESIAN_POINT('',(8.,-0.8,9.4));
#10323=CARTESIAN_POINT('',(8.,-0.8,9.4));
#10324=CARTESIAN_POINT('',(8.,-0.8,9.));
#10325=CARTESIAN_POINT('Origin',(-0.8,-0.8,9.));
#10326=CARTESIAN_POINT('',(-0.8,-0.8,9.));
#10327=CARTESIAN_POINT('',(-0.8,-0.8,9.));
#10328=CARTESIAN_POINT('',(-0.8,-0.8,9.4));
#10329=CARTESIAN_POINT('',(-0.8,-0.8,9.4));
#10330=CARTESIAN_POINT('',(-0.8,-0.8,9.));
#10331=CARTESIAN_POINT('Origin',(-0.8,0.8,9.));
#10332=CARTESIAN_POINT('',(-0.8,0.8,9.));
#10333=CARTESIAN_POINT('',(-0.8,0.8,9.4));
#10334=CARTESIAN_POINT('Origin',(3.6,0.,9.4));
#10335=CARTESIAN_POINT('Origin',(3.6,0.,9.));
#10336=CARTESIAN_POINT('',(0.,0.,0.));
#10337=CARTESIAN_POINT('Origin',(0.,0.,9.4));
#10338=CARTESIAN_POINT('',(-0.225,-2.75545529808154E-17,9.6));
#10339=CARTESIAN_POINT('Origin',(0.,0.,9.6));
#10340=CARTESIAN_POINT('',(-0.225,-2.75545529808154E-17,9.4));
#10341=CARTESIAN_POINT('',(-0.225,-2.75545529808154E-17,9.4));
#10342=CARTESIAN_POINT('Origin',(0.,0.,9.4));
#10343=CARTESIAN_POINT('Origin',(0.,0.,9.4));
#10344=CARTESIAN_POINT('',(-0.6,-7.34788079488412E-17,9.6));
#10345=CARTESIAN_POINT('Origin',(0.,0.,9.6));
#10346=CARTESIAN_POINT('',(-0.6,-7.34788079488412E-17,9.4));
#10347=CARTESIAN_POINT('',(-0.6,-7.34788079488412E-17,9.4));
#10348=CARTESIAN_POINT('Origin',(0.,0.,9.4));
#10349=CARTESIAN_POINT('Origin',(0.,0.,9.6));
#10350=CARTESIAN_POINT('Origin',(0.,0.,9.4));
#10351=CARTESIAN_POINT('',(0.,0.,0.));
#10352=CARTESIAN_POINT('Origin',(8.5,1.,9.4));
#10353=CARTESIAN_POINT('',(8.5,1.,9.4));
#10354=CARTESIAN_POINT('',(6.,1.,9.4));
#10355=CARTESIAN_POINT('',(8.5,1.,9.4));
#10356=CARTESIAN_POINT('',(6.,1.,10.2));
#10357=CARTESIAN_POINT('',(6.,1.,9.4));
#10358=CARTESIAN_POINT('',(8.5,1.,10.2));
#10359=CARTESIAN_POINT('',(8.5,1.,10.2));
#10360=CARTESIAN_POINT('',(8.5,1.,9.4));
#10361=CARTESIAN_POINT('Origin',(8.5,-1.,9.4));
#10362=CARTESIAN_POINT('',(8.5,-1.,9.4));
#10363=CARTESIAN_POINT('',(8.5,-1.,9.4));
#10364=CARTESIAN_POINT('',(8.5,-1.,10.2));
#10365=CARTESIAN_POINT('',(8.5,-1.,10.2));
#10366=CARTESIAN_POINT('',(8.5,-1.,9.4));
#10367=CARTESIAN_POINT('Origin',(6.,-1.,9.4));
#10368=CARTESIAN_POINT('',(6.,-1.,9.4));
#10369=CARTESIAN_POINT('',(6.,-1.,9.4));
#10370=CARTESIAN_POINT('',(6.,-1.,10.2));
#10371=CARTESIAN_POINT('',(6.,-1.,10.2));
#10372=CARTESIAN_POINT('',(6.,-1.,9.4));
#10373=CARTESIAN_POINT('Origin',(6.,1.,9.4));
#10374=CARTESIAN_POINT('',(6.,1.,9.4));
#10375=CARTESIAN_POINT('',(6.,1.,10.2));
#10376=CARTESIAN_POINT('Origin',(7.25,0.,10.2));
#10377=CARTESIAN_POINT('Origin',(7.25,0.,9.4));
#10378=CARTESIAN_POINT('',(0.,0.,0.));
#10379=CARTESIAN_POINT('Origin',(0.0866025403784439,-0.4,-0.15));
#10380=CARTESIAN_POINT('',(0.173205080756888,-0.4,0.));
#10381=CARTESIAN_POINT('',(0.0866025403784439,-0.4,-0.15));
#10382=CARTESIAN_POINT('',(0.173205080756888,-0.4,0.));
#10383=CARTESIAN_POINT('',(0.0866025403784439,-0.64,-0.15));
#10384=CARTESIAN_POINT('',(0.0866025403784439,-0.4,-0.15));
#10385=CARTESIAN_POINT('',(0.173205080756888,-0.64,0.));
#10386=CARTESIAN_POINT('',(0.173205080756888,-0.64,0.));
#10387=CARTESIAN_POINT('',(0.173205080756888,-0.4,0.));
#10388=CARTESIAN_POINT('Origin',(-0.0866025403784438,-0.4,-0.15));
#10389=CARTESIAN_POINT('',(-0.0866025403784438,-0.4,-0.15));
#10390=CARTESIAN_POINT('',(0.0866025403784439,-0.4,-0.15));
#10391=CARTESIAN_POINT('',(-0.0866025403784438,-0.64,-0.15));
#10392=CARTESIAN_POINT('',(-0.0866025403784438,-0.4,-0.15));
#10393=CARTESIAN_POINT('',(0.0866025403784439,-0.64,-0.15));
#10394=CARTESIAN_POINT('Origin',(-0.173205080756888,-0.4,-2.77555756156289E-17));
#10395=CARTESIAN_POINT('',(-0.173205080756888,-0.4,-2.12115047744981E-17));
#10396=CARTESIAN_POINT('',(-0.0866025403784438,-0.4,-0.15));
#10397=CARTESIAN_POINT('',(-0.173205080756888,-0.64,-2.77555756156289E-17));
#10398=CARTESIAN_POINT('',(-0.173205080756888,-0.4,-2.12115047744981E-17));
#10399=CARTESIAN_POINT('',(-0.0866025403784438,-0.64,-0.15));
#10400=CARTESIAN_POINT('Origin',(-0.0866025403784439,-0.4,0.15));
#10401=CARTESIAN_POINT('',(-0.0866025403784439,-0.4,0.15));
#10402=CARTESIAN_POINT('',(-0.173205080756888,-0.4,-2.12115047744981E-17));
#10403=CARTESIAN_POINT('',(-0.0866025403784439,-0.64,0.15));
#10404=CARTESIAN_POINT('',(-0.0866025403784439,-0.4,0.15));
#10405=CARTESIAN_POINT('',(-0.173205080756888,-0.64,-2.12115047744981E-17));
#10406=CARTESIAN_POINT('Origin',(0.0866025403784439,-0.4,0.15));
#10407=CARTESIAN_POINT('',(0.0866025403784439,-0.4,0.15));
#10408=CARTESIAN_POINT('',(-0.0866025403784439,-0.4,0.15));
#10409=CARTESIAN_POINT('',(0.0866025403784439,-0.64,0.15));
#10410=CARTESIAN_POINT('',(0.0866025403784439,-0.4,0.15));
#10411=CARTESIAN_POINT('',(-0.0866025403784439,-0.64,0.15));
#10412=CARTESIAN_POINT('Origin',(0.173205080756888,-0.4,0.));
#10413=CARTESIAN_POINT('',(0.0866025403784439,-0.4,0.15));
#10414=CARTESIAN_POINT('',(0.0866025403784439,-0.64,0.15));
#10415=CARTESIAN_POINT('Origin',(0.,-0.4,-2.77555756156289E-17));
#10416=CARTESIAN_POINT('Origin',(0.,-0.64,-2.77555756156289E-17));
#10417=CARTESIAN_POINT('Origin',(0.,-1.,0.));
#10418=CARTESIAN_POINT('',(-0.1954,-1.,2.39295984553393E-17));
#10419=CARTESIAN_POINT('Origin',(0.,-1.,0.));
#10420=CARTESIAN_POINT('Origin',(0.3,0.4,0.));
#10421=CARTESIAN_POINT('',(-0.3,0.4,-3.67394039744206E-17));
#10422=CARTESIAN_POINT('Origin',(0.,0.4,0.));
#10423=CARTESIAN_POINT('Origin',(0.,0.375,0.));
#10424=CARTESIAN_POINT('',(-0.35,0.35,-4.28626379701573E-17));
#10425=CARTESIAN_POINT('Origin',(0.,0.35,0.));
#10426=CARTESIAN_POINT('',(-0.325,0.375,-3.9801020972289E-17));
#10427=CARTESIAN_POINT('Origin',(0.,0.19,0.));
#10428=CARTESIAN_POINT('',(-0.35,0.03,-4.28626379701574E-17));
#10429=CARTESIAN_POINT('Origin',(0.,0.03,0.));
#10430=CARTESIAN_POINT('',(-0.35,0.19,-4.28626379701574E-17));
#10431=CARTESIAN_POINT('Origin',(0.,0.0149999999999999,0.));
#10432=CARTESIAN_POINT('',(-0.32,-3.29597460435593E-17,-3.91886975727153E-17));
#10433=CARTESIAN_POINT('Origin',(0.,0.,0.));
#10434=CARTESIAN_POINT('',(-0.335,0.0149999999999999,-4.10256677714363E-17));
#10435=CARTESIAN_POINT('Origin',(0.22,0.,0.));
#10436=CARTESIAN_POINT('',(-0.22,-6.93889390390723E-18,-2.69422295812418E-17));
#10437=CARTESIAN_POINT('Origin',(0.,0.,0.));
#10438=CARTESIAN_POINT('Origin',(0.,-0.02,0.));
#10439=CARTESIAN_POINT('',(-0.1954,-0.0492,2.39295984553393E-17));
#10440=CARTESIAN_POINT('Origin',(0.,-0.0492,0.));
#10441=CARTESIAN_POINT('',(-0.21,-0.02,-2.57175827820944E-17));
#10442=CARTESIAN_POINT('Origin',(0.,-0.8,0.));
#10443=CARTESIAN_POINT('',(-0.1954,-0.8,-2.39295984553393E-17));
#10444=CARTESIAN_POINT('',(0.,0.,0.));
#10445=CARTESIAN_POINT('',(0.,0.,0.));
#10446=CARTESIAN_POINT('',(0.,0.,0.));
#10447=CARTESIAN_POINT('',(0.,0.,0.));
#10448=CARTESIAN_POINT('',(0.,0.,0.));
#10449=CARTESIAN_POINT('',(0.,0.,9.6));
#10450=CARTESIAN_POINT('',(0.,0.,0.));
#10451=CARTESIAN_POINT('',(-3.06161699786839E-16,-2.75051632829333E-33,
-4.88498130835069E-15));
#10452=UNCERTAINTY_MEASURE_WITH_UNIT(LENGTH_MEASURE(0.001),#10518,
'DISTANCE_ACCURACY_VALUE',
'Maximum model space distance between geometric entities at asserted c
onnectivities');
#10453=UNCERTAINTY_MEASURE_WITH_UNIT(LENGTH_MEASURE(0.001),#10518,
'DISTANCE_ACCURACY_VALUE',
'Maximum model space distance between geometric entities at asserted c
onnectivities');
#10454=UNCERTAINTY_MEASURE_WITH_UNIT(LENGTH_MEASURE(0.001),#10518,
'DISTANCE_ACCURACY_VALUE',
'Maximum model space distance between geometric entities at asserted c
onnectivities');
#10455=UNCERTAINTY_MEASURE_WITH_UNIT(LENGTH_MEASURE(0.001),#10518,
'DISTANCE_ACCURACY_VALUE',
'Maximum model space distance between geometric entities at asserted c
onnectivities');
#10456=UNCERTAINTY_MEASURE_WITH_UNIT(LENGTH_MEASURE(0.001),#10518,
'DISTANCE_ACCURACY_VALUE',
'Maximum model space distance between geometric entities at asserted c
onnectivities');
#10457=UNCERTAINTY_MEASURE_WITH_UNIT(LENGTH_MEASURE(0.001),#10518,
'DISTANCE_ACCURACY_VALUE',
'Maximum model space distance between geometric entities at asserted c
onnectivities');
#10458=UNCERTAINTY_MEASURE_WITH_UNIT(LENGTH_MEASURE(0.001),#10518,
'DISTANCE_ACCURACY_VALUE',
'Maximum model space distance between geometric entities at asserted c
onnectivities');
#10459=UNCERTAINTY_MEASURE_WITH_UNIT(LENGTH_MEASURE(0.001),#10518,
'DISTANCE_ACCURACY_VALUE',
'Maximum model space distance between geometric entities at asserted c
onnectivities');
#10460=UNCERTAINTY_MEASURE_WITH_UNIT(LENGTH_MEASURE(0.001),#10518,
'DISTANCE_ACCURACY_VALUE',
'Maximum model space distance between geometric entities at asserted c
onnectivities');
#10461=UNCERTAINTY_MEASURE_WITH_UNIT(LENGTH_MEASURE(0.001),#10518,
'DISTANCE_ACCURACY_VALUE',
'Maximum model space distance between geometric entities at asserted c
onnectivities');
#10462=UNCERTAINTY_MEASURE_WITH_UNIT(LENGTH_MEASURE(0.001),#10518,
'DISTANCE_ACCURACY_VALUE',
'Maximum model space distance between geometric entities at asserted c
onnectivities');
#10463=UNCERTAINTY_MEASURE_WITH_UNIT(LENGTH_MEASURE(0.001),#10518,
'DISTANCE_ACCURACY_VALUE',
'Maximum model space distance between geometric entities at asserted c
onnectivities');
#10464=UNCERTAINTY_MEASURE_WITH_UNIT(LENGTH_MEASURE(0.001),#10518,
'DISTANCE_ACCURACY_VALUE',
'Maximum model space distance between geometric entities at asserted c
onnectivities');
#10465=UNCERTAINTY_MEASURE_WITH_UNIT(LENGTH_MEASURE(0.001),#10518,
'DISTANCE_ACCURACY_VALUE',
'Maximum model space distance between geometric entities at asserted c
onnectivities');
#10466=UNCERTAINTY_MEASURE_WITH_UNIT(LENGTH_MEASURE(0.001),#10518,
'DISTANCE_ACCURACY_VALUE',
'Maximum model space distance between geometric entities at asserted c
onnectivities');
#10467=UNCERTAINTY_MEASURE_WITH_UNIT(LENGTH_MEASURE(0.001),#10518,
'DISTANCE_ACCURACY_VALUE',
'Maximum model space distance between geometric entities at asserted c
onnectivities');
#10468=UNCERTAINTY_MEASURE_WITH_UNIT(LENGTH_MEASURE(0.001),#10518,
'DISTANCE_ACCURACY_VALUE',
'Maximum model space distance between geometric entities at asserted c
onnectivities');
#10469=UNCERTAINTY_MEASURE_WITH_UNIT(LENGTH_MEASURE(0.001),#10518,
'DISTANCE_ACCURACY_VALUE',
'Maximum model space distance between geometric entities at asserted c
onnectivities');
#10470=UNCERTAINTY_MEASURE_WITH_UNIT(LENGTH_MEASURE(0.001),#10518,
'DISTANCE_ACCURACY_VALUE',
'Maximum model space distance between geometric entities at asserted c
onnectivities');
#10471=UNCERTAINTY_MEASURE_WITH_UNIT(LENGTH_MEASURE(0.001),#10518,
'DISTANCE_ACCURACY_VALUE',
'Maximum model space distance between geometric entities at asserted c
onnectivities');
#10472=UNCERTAINTY_MEASURE_WITH_UNIT(LENGTH_MEASURE(0.001),#10518,
'DISTANCE_ACCURACY_VALUE',
'Maximum model space distance between geometric entities at asserted c
onnectivities');
#10473=UNCERTAINTY_MEASURE_WITH_UNIT(LENGTH_MEASURE(0.001),#10518,
'DISTANCE_ACCURACY_VALUE',
'Maximum model space distance between geometric entities at asserted c
onnectivities');
#10474=UNCERTAINTY_MEASURE_WITH_UNIT(LENGTH_MEASURE(0.001),#10518,
'DISTANCE_ACCURACY_VALUE',
'Maximum model space distance between geometric entities at asserted c
onnectivities');
#10475=UNCERTAINTY_MEASURE_WITH_UNIT(LENGTH_MEASURE(0.001),#10518,
'DISTANCE_ACCURACY_VALUE',
'Maximum model space distance between geometric entities at asserted c
onnectivities');
#10476=UNCERTAINTY_MEASURE_WITH_UNIT(LENGTH_MEASURE(0.001),#10518,
'DISTANCE_ACCURACY_VALUE',
'Maximum model space distance between geometric entities at asserted c
onnectivities');
#10477=UNCERTAINTY_MEASURE_WITH_UNIT(LENGTH_MEASURE(0.001),#10518,
'DISTANCE_ACCURACY_VALUE',
'Maximum model space distance between geometric entities at asserted c
onnectivities');
#10478=UNCERTAINTY_MEASURE_WITH_UNIT(LENGTH_MEASURE(0.001),#10518,
'DISTANCE_ACCURACY_VALUE',
'Maximum model space distance between geometric entities at asserted c
onnectivities');
#10479=UNCERTAINTY_MEASURE_WITH_UNIT(LENGTH_MEASURE(0.001),#10518,
'DISTANCE_ACCURACY_VALUE',
'Maximum model space distance between geometric entities at asserted c
onnectivities');
#10480=UNCERTAINTY_MEASURE_WITH_UNIT(LENGTH_MEASURE(0.001),#10518,
'DISTANCE_ACCURACY_VALUE',
'Maximum model space distance between geometric entities at asserted c
onnectivities');
#10481=UNCERTAINTY_MEASURE_WITH_UNIT(LENGTH_MEASURE(0.001),#10518,
'DISTANCE_ACCURACY_VALUE',
'Maximum model space distance between geometric entities at asserted c
onnectivities');
#10482=UNCERTAINTY_MEASURE_WITH_UNIT(LENGTH_MEASURE(0.001),#10518,
'DISTANCE_ACCURACY_VALUE',
'Maximum model space distance between geometric entities at asserted c
onnectivities');
#10483=UNCERTAINTY_MEASURE_WITH_UNIT(LENGTH_MEASURE(0.001),#10518,
'DISTANCE_ACCURACY_VALUE',
'Maximum model space distance between geometric entities at asserted c
onnectivities');
#10484=UNCERTAINTY_MEASURE_WITH_UNIT(LENGTH_MEASURE(0.001),#10518,
'DISTANCE_ACCURACY_VALUE',
'Maximum model space distance between geometric entities at asserted c
onnectivities');
#10485=(
GEOMETRIC_REPRESENTATION_CONTEXT(3)
GLOBAL_UNCERTAINTY_ASSIGNED_CONTEXT((#10452))
GLOBAL_UNIT_ASSIGNED_CONTEXT((#10518,#10520,#10521))
REPRESENTATION_CONTEXT('','3D')
);
#10486=(
GEOMETRIC_REPRESENTATION_CONTEXT(3)
GLOBAL_UNCERTAINTY_ASSIGNED_CONTEXT((#10453))
GLOBAL_UNIT_ASSIGNED_CONTEXT((#10518,#10520,#10521))
REPRESENTATION_CONTEXT('','3D')
);
#10487=(
GEOMETRIC_REPRESENTATION_CONTEXT(3)
GLOBAL_UNCERTAINTY_ASSIGNED_CONTEXT((#10454))
GLOBAL_UNIT_ASSIGNED_CONTEXT((#10518,#10520,#10521))
REPRESENTATION_CONTEXT('','3D')
);
#10488=(
GEOMETRIC_REPRESENTATION_CONTEXT(3)
GLOBAL_UNCERTAINTY_ASSIGNED_CONTEXT((#10455))
GLOBAL_UNIT_ASSIGNED_CONTEXT((#10518,#10520,#10521))
REPRESENTATION_CONTEXT('','3D')
);
#10489=(
GEOMETRIC_REPRESENTATION_CONTEXT(3)
GLOBAL_UNCERTAINTY_ASSIGNED_CONTEXT((#10456))
GLOBAL_UNIT_ASSIGNED_CONTEXT((#10518,#10520,#10521))
REPRESENTATION_CONTEXT('','3D')
);
#10490=(
GEOMETRIC_REPRESENTATION_CONTEXT(3)
GLOBAL_UNCERTAINTY_ASSIGNED_CONTEXT((#10457))
GLOBAL_UNIT_ASSIGNED_CONTEXT((#10518,#10520,#10521))
REPRESENTATION_CONTEXT('','3D')
);
#10491=(
GEOMETRIC_REPRESENTATION_CONTEXT(3)
GLOBAL_UNCERTAINTY_ASSIGNED_CONTEXT((#10458))
GLOBAL_UNIT_ASSIGNED_CONTEXT((#10518,#10520,#10521))
REPRESENTATION_CONTEXT('','3D')
);
#10492=(
GEOMETRIC_REPRESENTATION_CONTEXT(3)
GLOBAL_UNCERTAINTY_ASSIGNED_CONTEXT((#10459))
GLOBAL_UNIT_ASSIGNED_CONTEXT((#10518,#10520,#10521))
REPRESENTATION_CONTEXT('','3D')
);
#10493=(
GEOMETRIC_REPRESENTATION_CONTEXT(3)
GLOBAL_UNCERTAINTY_ASSIGNED_CONTEXT((#10460))
GLOBAL_UNIT_ASSIGNED_CONTEXT((#10518,#10520,#10521))
REPRESENTATION_CONTEXT('','3D')
);
#10494=(
GEOMETRIC_REPRESENTATION_CONTEXT(3)
GLOBAL_UNCERTAINTY_ASSIGNED_CONTEXT((#10461))
GLOBAL_UNIT_ASSIGNED_CONTEXT((#10518,#10520,#10521))
REPRESENTATION_CONTEXT('','3D')
);
#10495=(
GEOMETRIC_REPRESENTATION_CONTEXT(3)
GLOBAL_UNCERTAINTY_ASSIGNED_CONTEXT((#10462))
GLOBAL_UNIT_ASSIGNED_CONTEXT((#10518,#10520,#10521))
REPRESENTATION_CONTEXT('','3D')
);
#10496=(
GEOMETRIC_REPRESENTATION_CONTEXT(3)
GLOBAL_UNCERTAINTY_ASSIGNED_CONTEXT((#10463))
GLOBAL_UNIT_ASSIGNED_CONTEXT((#10518,#10520,#10521))
REPRESENTATION_CONTEXT('','3D')
);
#10497=(
GEOMETRIC_REPRESENTATION_CONTEXT(3)
GLOBAL_UNCERTAINTY_ASSIGNED_CONTEXT((#10464))
GLOBAL_UNIT_ASSIGNED_CONTEXT((#10518,#10520,#10521))
REPRESENTATION_CONTEXT('','3D')
);
#10498=(
GEOMETRIC_REPRESENTATION_CONTEXT(3)
GLOBAL_UNCERTAINTY_ASSIGNED_CONTEXT((#10465))
GLOBAL_UNIT_ASSIGNED_CONTEXT((#10518,#10520,#10521))
REPRESENTATION_CONTEXT('','3D')
);
#10499=(
GEOMETRIC_REPRESENTATION_CONTEXT(3)
GLOBAL_UNCERTAINTY_ASSIGNED_CONTEXT((#10466))
GLOBAL_UNIT_ASSIGNED_CONTEXT((#10518,#10520,#10521))
REPRESENTATION_CONTEXT('','3D')
);
#10500=(
GEOMETRIC_REPRESENTATION_CONTEXT(3)
GLOBAL_UNCERTAINTY_ASSIGNED_CONTEXT((#10467))
GLOBAL_UNIT_ASSIGNED_CONTEXT((#10518,#10520,#10521))
REPRESENTATION_CONTEXT('','3D')
);
#10501=(
GEOMETRIC_REPRESENTATION_CONTEXT(3)
GLOBAL_UNCERTAINTY_ASSIGNED_CONTEXT((#10468))
GLOBAL_UNIT_ASSIGNED_CONTEXT((#10518,#10520,#10521))
REPRESENTATION_CONTEXT('','3D')
);
#10502=(
GEOMETRIC_REPRESENTATION_CONTEXT(3)
GLOBAL_UNCERTAINTY_ASSIGNED_CONTEXT((#10469))
GLOBAL_UNIT_ASSIGNED_CONTEXT((#10518,#10520,#10521))
REPRESENTATION_CONTEXT('','3D')
);
#10503=(
GEOMETRIC_REPRESENTATION_CONTEXT(3)
GLOBAL_UNCERTAINTY_ASSIGNED_CONTEXT((#10470))
GLOBAL_UNIT_ASSIGNED_CONTEXT((#10518,#10520,#10521))
REPRESENTATION_CONTEXT('','3D')
);
#10504=(
GEOMETRIC_REPRESENTATION_CONTEXT(3)
GLOBAL_UNCERTAINTY_ASSIGNED_CONTEXT((#10471))
GLOBAL_UNIT_ASSIGNED_CONTEXT((#10518,#10520,#10521))
REPRESENTATION_CONTEXT('','3D')
);
#10505=(
GEOMETRIC_REPRESENTATION_CONTEXT(3)
GLOBAL_UNCERTAINTY_ASSIGNED_CONTEXT((#10472))
GLOBAL_UNIT_ASSIGNED_CONTEXT((#10518,#10520,#10521))
REPRESENTATION_CONTEXT('','3D')
);
#10506=(
GEOMETRIC_REPRESENTATION_CONTEXT(3)
GLOBAL_UNCERTAINTY_ASSIGNED_CONTEXT((#10473))
GLOBAL_UNIT_ASSIGNED_CONTEXT((#10518,#10520,#10521))
REPRESENTATION_CONTEXT('','3D')
);
#10507=(
GEOMETRIC_REPRESENTATION_CONTEXT(3)
GLOBAL_UNCERTAINTY_ASSIGNED_CONTEXT((#10474))
GLOBAL_UNIT_ASSIGNED_CONTEXT((#10518,#10520,#10521))
REPRESENTATION_CONTEXT('','3D')
);
#10508=(
GEOMETRIC_REPRESENTATION_CONTEXT(3)
GLOBAL_UNCERTAINTY_ASSIGNED_CONTEXT((#10475))
GLOBAL_UNIT_ASSIGNED_CONTEXT((#10518,#10520,#10521))
REPRESENTATION_CONTEXT('','3D')
);
#10509=(
GEOMETRIC_REPRESENTATION_CONTEXT(3)
GLOBAL_UNCERTAINTY_ASSIGNED_CONTEXT((#10476))
GLOBAL_UNIT_ASSIGNED_CONTEXT((#10518,#10520,#10521))
REPRESENTATION_CONTEXT('','3D')
);
#10510=(
GEOMETRIC_REPRESENTATION_CONTEXT(3)
GLOBAL_UNCERTAINTY_ASSIGNED_CONTEXT((#10477))
GLOBAL_UNIT_ASSIGNED_CONTEXT((#10518,#10520,#10521))
REPRESENTATION_CONTEXT('','3D')
);
#10511=(
GEOMETRIC_REPRESENTATION_CONTEXT(3)
GLOBAL_UNCERTAINTY_ASSIGNED_CONTEXT((#10478))
GLOBAL_UNIT_ASSIGNED_CONTEXT((#10518,#10520,#10521))
REPRESENTATION_CONTEXT('','3D')
);
#10512=(
GEOMETRIC_REPRESENTATION_CONTEXT(3)
GLOBAL_UNCERTAINTY_ASSIGNED_CONTEXT((#10479))
GLOBAL_UNIT_ASSIGNED_CONTEXT((#10518,#10520,#10521))
REPRESENTATION_CONTEXT('','3D')
);
#10513=(
GEOMETRIC_REPRESENTATION_CONTEXT(3)
GLOBAL_UNCERTAINTY_ASSIGNED_CONTEXT((#10480))
GLOBAL_UNIT_ASSIGNED_CONTEXT((#10518,#10520,#10521))
REPRESENTATION_CONTEXT('','3D')
);
#10514=(
GEOMETRIC_REPRESENTATION_CONTEXT(3)
GLOBAL_UNCERTAINTY_ASSIGNED_CONTEXT((#10481))
GLOBAL_UNIT_ASSIGNED_CONTEXT((#10518,#10520,#10521))
REPRESENTATION_CONTEXT('','3D')
);
#10515=(
GEOMETRIC_REPRESENTATION_CONTEXT(3)
GLOBAL_UNCERTAINTY_ASSIGNED_CONTEXT((#10482))
GLOBAL_UNIT_ASSIGNED_CONTEXT((#10518,#10520,#10521))
REPRESENTATION_CONTEXT('','3D')
);
#10516=(
GEOMETRIC_REPRESENTATION_CONTEXT(3)
GLOBAL_UNCERTAINTY_ASSIGNED_CONTEXT((#10483))
GLOBAL_UNIT_ASSIGNED_CONTEXT((#10518,#10520,#10521))
REPRESENTATION_CONTEXT('','3D')
);
#10517=(
GEOMETRIC_REPRESENTATION_CONTEXT(3)
GLOBAL_UNCERTAINTY_ASSIGNED_CONTEXT((#10484))
GLOBAL_UNIT_ASSIGNED_CONTEXT((#10518,#10520,#10521))
REPRESENTATION_CONTEXT('','3D')
);
#10518=(
LENGTH_UNIT()
NAMED_UNIT(*)
SI_UNIT(.CENTI.,.METRE.)
);
#10519=(
LENGTH_UNIT()
NAMED_UNIT(*)
SI_UNIT($,.METRE.)
);
#10520=(
NAMED_UNIT(*)
PLANE_ANGLE_UNIT()
SI_UNIT($,.RADIAN.)
);
#10521=(
NAMED_UNIT(*)
SI_UNIT($,.STERADIAN.)
SOLID_ANGLE_UNIT()
);
#10522=SHAPE_DEFINITION_REPRESENTATION(#10554,#10641);
#10523=SHAPE_DEFINITION_REPRESENTATION(#10555,#10642);
#10524=SHAPE_DEFINITION_REPRESENTATION(#10556,#10643);
#10525=SHAPE_DEFINITION_REPRESENTATION(#10557,#10644);
#10526=SHAPE_DEFINITION_REPRESENTATION(#10558,#10645);
#10527=SHAPE_DEFINITION_REPRESENTATION(#10559,#10646);
#10528=SHAPE_DEFINITION_REPRESENTATION(#10560,#10647);
#10529=SHAPE_DEFINITION_REPRESENTATION(#10561,#10648);
#10530=SHAPE_DEFINITION_REPRESENTATION(#10562,#10649);
#10531=SHAPE_DEFINITION_REPRESENTATION(#10563,#10650);
#10532=SHAPE_DEFINITION_REPRESENTATION(#10564,#10651);
#10533=SHAPE_DEFINITION_REPRESENTATION(#10565,#10652);
#10534=SHAPE_DEFINITION_REPRESENTATION(#10566,#10653);
#10535=SHAPE_DEFINITION_REPRESENTATION(#10567,#10654);
#10536=SHAPE_DEFINITION_REPRESENTATION(#10568,#10655);
#10537=SHAPE_DEFINITION_REPRESENTATION(#10569,#10656);
#10538=SHAPE_DEFINITION_REPRESENTATION(#10570,#10657);
#10539=SHAPE_DEFINITION_REPRESENTATION(#10571,#10658);
#10540=SHAPE_DEFINITION_REPRESENTATION(#10572,#10659);
#10541=SHAPE_DEFINITION_REPRESENTATION(#10573,#10660);
#10542=SHAPE_DEFINITION_REPRESENTATION(#10574,#10661);
#10543=SHAPE_DEFINITION_REPRESENTATION(#10575,#10662);
#10544=SHAPE_DEFINITION_REPRESENTATION(#10576,#10663);
#10545=SHAPE_DEFINITION_REPRESENTATION(#10577,#10664);
#10546=SHAPE_DEFINITION_REPRESENTATION(#10578,#10665);
#10547=SHAPE_DEFINITION_REPRESENTATION(#10626,#10666);
#10548=SHAPE_DEFINITION_REPRESENTATION(#10627,#10667);
#10549=SHAPE_DEFINITION_REPRESENTATION(#10628,#10668);
#10550=SHAPE_DEFINITION_REPRESENTATION(#10629,#10669);
#10551=SHAPE_DEFINITION_REPRESENTATION(#10630,#10670);
#10552=SHAPE_DEFINITION_REPRESENTATION(#10631,#10671);
#10553=SHAPE_DEFINITION_REPRESENTATION(#10632,#10672);
#10554=PRODUCT_DEFINITION_SHAPE('',$,#10674);
#10555=PRODUCT_DEFINITION_SHAPE('',$,#10675);
#10556=PRODUCT_DEFINITION_SHAPE('',$,#10676);
#10557=PRODUCT_DEFINITION_SHAPE('',$,#10677);
#10558=PRODUCT_DEFINITION_SHAPE('',$,#10678);
#10559=PRODUCT_DEFINITION_SHAPE('',$,#10679);
#10560=PRODUCT_DEFINITION_SHAPE('',$,#10680);
#10561=PRODUCT_DEFINITION_SHAPE('',$,#10681);
#10562=PRODUCT_DEFINITION_SHAPE('',$,#10682);
#10563=PRODUCT_DEFINITION_SHAPE('',$,#10683);
#10564=PRODUCT_DEFINITION_SHAPE('',$,#10684);
#10565=PRODUCT_DEFINITION_SHAPE('',$,#10685);
#10566=PRODUCT_DEFINITION_SHAPE('',$,#10686);
#10567=PRODUCT_DEFINITION_SHAPE('',$,#10687);
#10568=PRODUCT_DEFINITION_SHAPE('',$,#10688);
#10569=PRODUCT_DEFINITION_SHAPE('',$,#10689);
#10570=PRODUCT_DEFINITION_SHAPE('',$,#10690);
#10571=PRODUCT_DEFINITION_SHAPE('',$,#10691);
#10572=PRODUCT_DEFINITION_SHAPE('',$,#10692);
#10573=PRODUCT_DEFINITION_SHAPE('',$,#10693);
#10574=PRODUCT_DEFINITION_SHAPE('',$,#10694);
#10575=PRODUCT_DEFINITION_SHAPE('',$,#10695);
#10576=PRODUCT_DEFINITION_SHAPE('',$,#10696);
#10577=PRODUCT_DEFINITION_SHAPE('',$,#10697);
#10578=PRODUCT_DEFINITION_SHAPE('',$,#10698);
#10579=PRODUCT_DEFINITION_SHAPE($,$,#176);
#10580=PRODUCT_DEFINITION_SHAPE($,$,#177);
#10581=PRODUCT_DEFINITION_SHAPE($,$,#178);
#10582=PRODUCT_DEFINITION_SHAPE($,$,#179);
#10583=PRODUCT_DEFINITION_SHAPE($,$,#180);
#10584=PRODUCT_DEFINITION_SHAPE($,$,#181);
#10585=PRODUCT_DEFINITION_SHAPE($,$,#182);
#10586=PRODUCT_DEFINITION_SHAPE($,$,#183);
#10587=PRODUCT_DEFINITION_SHAPE($,$,#184);
#10588=PRODUCT_DEFINITION_SHAPE($,$,#185);
#10589=PRODUCT_DEFINITION_SHAPE($,$,#186);
#10590=PRODUCT_DEFINITION_SHAPE($,$,#187);
#10591=PRODUCT_DEFINITION_SHAPE($,$,#188);
#10592=PRODUCT_DEFINITION_SHAPE($,$,#189);
#10593=PRODUCT_DEFINITION_SHAPE($,$,#190);
#10594=PRODUCT_DEFINITION_SHAPE($,$,#191);
#10595=PRODUCT_DEFINITION_SHAPE($,$,#192);
#10596=PRODUCT_DEFINITION_SHAPE($,$,#193);
#10597=PRODUCT_DEFINITION_SHAPE($,$,#194);
#10598=PRODUCT_DEFINITION_SHAPE($,$,#195);
#10599=PRODUCT_DEFINITION_SHAPE($,$,#196);
#10600=PRODUCT_DEFINITION_SHAPE($,$,#197);
#10601=PRODUCT_DEFINITION_SHAPE($,$,#198);
#10602=PRODUCT_DEFINITION_SHAPE($,$,#199);
#10603=PRODUCT_DEFINITION_SHAPE($,$,#200);
#10604=PRODUCT_DEFINITION_SHAPE($,$,#201);
#10605=PRODUCT_DEFINITION_SHAPE($,$,#202);
#10606=PRODUCT_DEFINITION_SHAPE($,$,#203);
#10607=PRODUCT_DEFINITION_SHAPE($,$,#204);
#10608=PRODUCT_DEFINITION_SHAPE($,$,#205);
#10609=PRODUCT_DEFINITION_SHAPE($,$,#206);
#10610=PRODUCT_DEFINITION_SHAPE($,$,#207);
#10611=PRODUCT_DEFINITION_SHAPE($,$,#208);
#10612=PRODUCT_DEFINITION_SHAPE($,$,#209);
#10613=PRODUCT_DEFINITION_SHAPE($,$,#210);
#10614=PRODUCT_DEFINITION_SHAPE($,$,#211);
#10615=PRODUCT_DEFINITION_SHAPE($,$,#212);
#10616=PRODUCT_DEFINITION_SHAPE($,$,#213);
#10617=PRODUCT_DEFINITION_SHAPE($,$,#214);
#10618=PRODUCT_DEFINITION_SHAPE($,$,#215);
#10619=PRODUCT_DEFINITION_SHAPE($,$,#216);
#10620=PRODUCT_DEFINITION_SHAPE($,$,#217);
#10621=PRODUCT_DEFINITION_SHAPE($,$,#218);
#10622=PRODUCT_DEFINITION_SHAPE($,$,#219);
#10623=PRODUCT_DEFINITION_SHAPE($,$,#220);
#10624=PRODUCT_DEFINITION_SHAPE($,$,#221);
#10625=PRODUCT_DEFINITION_SHAPE($,$,#222);
#10626=PRODUCT_DEFINITION_SHAPE('',$,#10699);
#10627=PRODUCT_DEFINITION_SHAPE('',$,#10700);
#10628=PRODUCT_DEFINITION_SHAPE('',$,#10701);
#10629=PRODUCT_DEFINITION_SHAPE('',$,#10702);
#10630=PRODUCT_DEFINITION_SHAPE('',$,#10703);
#10631=PRODUCT_DEFINITION_SHAPE('',$,#10704);
#10632=PRODUCT_DEFINITION_SHAPE('',$,#10705);
#10633=PRODUCT_DEFINITION_SHAPE($,$,#223);
#10634=PRODUCT_DEFINITION_SHAPE($,$,#224);
#10635=PRODUCT_DEFINITION_SHAPE($,$,#225);
#10636=PRODUCT_DEFINITION_SHAPE($,$,#226);
#10637=PRODUCT_DEFINITION_SHAPE($,$,#227);
#10638=PRODUCT_DEFINITION_SHAPE($,$,#228);
#10639=PRODUCT_DEFINITION_SHAPE($,$,#229);
#10640=PRODUCT_DEFINITION_SHAPE($,$,#230);
#10641=SHAPE_REPRESENTATION('',(#6235,#6922,#6923),#10485);
#10642=SHAPE_REPRESENTATION('',(#6236,#6766,#6767,#6768,#6769,#6770,#6771,
#6772,#6773,#6774,#6775,#6776,#6777,#6778,#6779,#6780,#6781,#6782,#6783,
#6784,#6785,#6786,#6787,#6788,#6789,#6790,#6791,#6792,#6793,#6794,#6795,
#6796,#6797,#6798,#6799,#6800,#6801,#6802,#6803,#6804,#6805,#6806,#6807,
#6808,#6809,#6810,#6811,#6812),#10486);
#10643=SHAPE_REPRESENTATION('',(#6237),#10487);
#10644=SHAPE_REPRESENTATION('',(#6254),#10488);
#10645=SHAPE_REPRESENTATION('',(#6271),#10489);
#10646=SHAPE_REPRESENTATION('',(#6333),#10490);
#10647=SHAPE_REPRESENTATION('',(#6345),#10491);
#10648=SHAPE_REPRESENTATION('',(#6381),#10492);
#10649=SHAPE_REPRESENTATION('',(#6424),#10493);
#10650=SHAPE_REPRESENTATION('',(#6467),#10494);
#10651=SHAPE_REPRESENTATION('',(#6494),#10495);
#10652=SHAPE_REPRESENTATION('',(#6507),#10496);
#10653=SHAPE_REPRESENTATION('',(#6511),#10497);
#10654=SHAPE_REPRESENTATION('',(#6524),#10498);
#10655=SHAPE_REPRESENTATION('',(#6554),#10499);
#10656=SHAPE_REPRESENTATION('',(#6565),#10500);
#10657=SHAPE_REPRESENTATION('',(#6593),#10501);
#10658=SHAPE_REPRESENTATION('',(#6604),#10502);
#10659=SHAPE_REPRESENTATION('',(#6620),#10503);
#10660=SHAPE_REPRESENTATION('',(#6644),#10504);
#10661=SHAPE_REPRESENTATION('',(#6653),#10505);
#10662=SHAPE_REPRESENTATION('',(#6679),#10506);
#10663=SHAPE_REPRESENTATION('',(#6685),#10507);
#10664=SHAPE_REPRESENTATION('',(#6725),#10508);
#10665=SHAPE_REPRESENTATION('',(#6749),#10509);
#10666=SHAPE_REPRESENTATION('',(#6813,#6916,#6917,#6918,#6919,#6920,#6921),
#10510);
#10667=SHAPE_REPRESENTATION('',(#6814),#10511);
#10668=SHAPE_REPRESENTATION('',(#6830),#10512);
#10669=SHAPE_REPRESENTATION('',(#6865),#10513);
#10670=SHAPE_REPRESENTATION('',(#6876),#10514);
#10671=SHAPE_REPRESENTATION('',(#6885),#10515);
#10672=SHAPE_REPRESENTATION('',(#6892),#10516);
#10673=PRODUCT_DEFINITION_CONTEXT('part definition',#10771,'design');
#10674=PRODUCT_DEFINITION('PAT-121','PAT-121',#10706,
#10673);
#10675=PRODUCT_DEFINITION('Bracket pipework and valve body',
'Bracket pipework and valve body',#10707,#10673);
#10676=PRODUCT_DEFINITION('Valve port reducer','Valve port reducer',#10708,
#10673);
#10677=PRODUCT_DEFINITION('Valve port reducer (1)',
'Valve port reducer (1)',#10709,#10673);
#10678=PRODUCT_DEFINITION('Wall bracket','Wall bracket',#10710,#10673);
#10679=PRODUCT_DEFINITION('Bulkhead retaining nut',
'Bulkhead retaining nut',#10711,#10673);
#10680=PRODUCT_DEFINITION('Hose barb','Hose barb',#10712,#10673);
#10681=PRODUCT_DEFINITION('Body inlet half','Body inlet half',#10713,#10673);
#10682=PRODUCT_DEFINITION('Body outlet half','Body outlet half',#10714,
#10673);
#10683=PRODUCT_DEFINITION('Split-body gasket','Split-body gasket',#10715,
#10673);
#10684=PRODUCT_DEFINITION('Stem guide','Stem guide',#10716,#10673);
#10685=PRODUCT_DEFINITION('Packing ring','Packing ring',#10717,#10673);
#10686=PRODUCT_DEFINITION('Packing retainer','Packing retainer',#10718,
#10673);
#10687=PRODUCT_DEFINITION('Lever stop bridge','Lever stop bridge',#10719,
#10673);
#10688=PRODUCT_DEFINITION('Ball seat','Ball seat',#10720,#10673);
#10689=PRODUCT_DEFINITION('M5x70 body screw','M5x70 body screw',#10721,
#10673);
#10690=PRODUCT_DEFINITION('Flat Washer - M5','Flat Washer - M5',#10722,
#10673);
#10691=PRODUCT_DEFINITION('Hex Nut - M5','Hex Nut - M5',#10723,#10673);
#10692=PRODUCT_DEFINITION(
'Hex Pipe Nipple - 1-2 Inch Tapered Pipe Thread',
'Hex Pipe Nipple - 1-2 Inch Tapered Pipe Thread',#10724,#10673);
#10693=PRODUCT_DEFINITION('Bridge spacer','Bridge spacer',#10725,#10673);
#10694=PRODUCT_DEFINITION('Cap Screw - M4x16','Cap Screw - M4x16',#10726,
#10673);
#10695=PRODUCT_DEFINITION('Stop pin','Stop pin',#10727,#10673);
#10696=PRODUCT_DEFINITION('Connected quarter-inch elbow',
'Connected quarter-inch elbow',#10728,#10673);
#10697=PRODUCT_DEFINITION(
'Hex Pipe Nipple - 1-4 Inch Tapered Pipe Thread',
'Hex Pipe Nipple - 1-4 Inch Tapered Pipe Thread',#10729,#10673);
#10698=PRODUCT_DEFINITION('Hex Bolt - M6 x 30 mm',
'Hex Bolt - M6 x 30 mm',#10730,#10673);
#10699=PRODUCT_DEFINITION('Valve ball stem and lever',
'Valve ball stem and lever',#10731,#10673);
#10700=PRODUCT_DEFINITION('Ported ball','Ported ball',#10732,#10673);
#10701=PRODUCT_DEFINITION('Stem','Stem',#10733,#10673);
#10702=PRODUCT_DEFINITION('Lever','Lever',#10734,#10673);
#10703=PRODUCT_DEFINITION('Lever keeper','Lever keeper',#10735,#10673);
#10704=PRODUCT_DEFINITION('Bonded grip','Bonded grip',#10736,#10673);
#10705=PRODUCT_DEFINITION('M4x10 Cap Screw','M4x10 Cap Screw',#10737,#10673);
#10706=PRODUCT_DEFINITION_FORMATION('',$,#10773);
#10707=PRODUCT_DEFINITION_FORMATION('',$,#10774);
#10708=PRODUCT_DEFINITION_FORMATION('',$,#10775);
#10709=PRODUCT_DEFINITION_FORMATION('',$,#10776);
#10710=PRODUCT_DEFINITION_FORMATION('',$,#10777);
#10711=PRODUCT_DEFINITION_FORMATION('',$,#10778);
#10712=PRODUCT_DEFINITION_FORMATION('',$,#10779);
#10713=PRODUCT_DEFINITION_FORMATION('',$,#10780);
#10714=PRODUCT_DEFINITION_FORMATION('',$,#10781);
#10715=PRODUCT_DEFINITION_FORMATION('',$,#10782);
#10716=PRODUCT_DEFINITION_FORMATION('',$,#10783);
#10717=PRODUCT_DEFINITION_FORMATION('',$,#10784);
#10718=PRODUCT_DEFINITION_FORMATION('',$,#10785);
#10719=PRODUCT_DEFINITION_FORMATION('',$,#10786);
#10720=PRODUCT_DEFINITION_FORMATION('',$,#10787);
#10721=PRODUCT_DEFINITION_FORMATION('',$,#10788);
#10722=PRODUCT_DEFINITION_FORMATION('',$,#10789);
#10723=PRODUCT_DEFINITION_FORMATION('',$,#10790);
#10724=PRODUCT_DEFINITION_FORMATION('',$,#10791);
#10725=PRODUCT_DEFINITION_FORMATION('',$,#10792);
#10726=PRODUCT_DEFINITION_FORMATION('',$,#10793);
#10727=PRODUCT_DEFINITION_FORMATION('',$,#10794);
#10728=PRODUCT_DEFINITION_FORMATION('',$,#10795);
#10729=PRODUCT_DEFINITION_FORMATION('',$,#10796);
#10730=PRODUCT_DEFINITION_FORMATION('',$,#10797);
#10731=PRODUCT_DEFINITION_FORMATION('',$,#10798);
#10732=PRODUCT_DEFINITION_FORMATION('',$,#10799);
#10733=PRODUCT_DEFINITION_FORMATION('',$,#10800);
#10734=PRODUCT_DEFINITION_FORMATION('',$,#10801);
#10735=PRODUCT_DEFINITION_FORMATION('',$,#10802);
#10736=PRODUCT_DEFINITION_FORMATION('',$,#10803);
#10737=PRODUCT_DEFINITION_FORMATION('',$,#10804);
#10738=PRODUCT_RELATED_PRODUCT_CATEGORY('PAT-121','PAT-121',(#10773));
#10739=PRODUCT_RELATED_PRODUCT_CATEGORY(
'Bracket pipework and valve body','Bracket pipework and valve body',(#10774));
#10740=PRODUCT_RELATED_PRODUCT_CATEGORY('Valve port reducer',
'Valve port reducer',(#10775));
#10741=PRODUCT_RELATED_PRODUCT_CATEGORY('Valve port reducer (1)',
'Valve port reducer (1)',(#10776));
#10742=PRODUCT_RELATED_PRODUCT_CATEGORY('Wall bracket','Wall bracket',(#10777));
#10743=PRODUCT_RELATED_PRODUCT_CATEGORY('Bulkhead retaining nut',
'Bulkhead retaining nut',(#10778));
#10744=PRODUCT_RELATED_PRODUCT_CATEGORY('Hose barb','Hose barb',(#10779));
#10745=PRODUCT_RELATED_PRODUCT_CATEGORY('Body inlet half',
'Body inlet half',(#10780));
#10746=PRODUCT_RELATED_PRODUCT_CATEGORY('Body outlet half',
'Body outlet half',(#10781));
#10747=PRODUCT_RELATED_PRODUCT_CATEGORY('Split-body gasket',
'Split-body gasket',(#10782));
#10748=PRODUCT_RELATED_PRODUCT_CATEGORY('Stem guide','Stem guide',(#10783));
#10749=PRODUCT_RELATED_PRODUCT_CATEGORY('Packing ring','Packing ring',(#10784));
#10750=PRODUCT_RELATED_PRODUCT_CATEGORY('Packing retainer',
'Packing retainer',(#10785));
#10751=PRODUCT_RELATED_PRODUCT_CATEGORY('Lever stop bridge',
'Lever stop bridge',(#10786));
#10752=PRODUCT_RELATED_PRODUCT_CATEGORY('Ball seat','Ball seat',(#10787));
#10753=PRODUCT_RELATED_PRODUCT_CATEGORY('M5x70 body screw',
'M5x70 body screw',(#10788));
#10754=PRODUCT_RELATED_PRODUCT_CATEGORY('Flat Washer - M5',
'Flat Washer - M5',(#10789));
#10755=PRODUCT_RELATED_PRODUCT_CATEGORY('Hex Nut - M5','Hex Nut - M5',(#10790));
#10756=PRODUCT_RELATED_PRODUCT_CATEGORY(
'Hex Pipe Nipple - 1-2 Inch Tapered Pipe Thread',
'Hex Pipe Nipple - 1-2 Inch Tapered Pipe Thread',(#10791));
#10757=PRODUCT_RELATED_PRODUCT_CATEGORY('Bridge spacer','Bridge spacer',
(#10792));
#10758=PRODUCT_RELATED_PRODUCT_CATEGORY('Cap Screw - M4x16',
'Cap Screw - M4x16',(#10793));
#10759=PRODUCT_RELATED_PRODUCT_CATEGORY('Stop pin','Stop pin',(#10794));
#10760=PRODUCT_RELATED_PRODUCT_CATEGORY('Connected quarter-inch elbow',
'Connected quarter-inch elbow',(#10795));
#10761=PRODUCT_RELATED_PRODUCT_CATEGORY(
'Hex Pipe Nipple - 1-4 Inch Tapered Pipe Thread',
'Hex Pipe Nipple - 1-4 Inch Tapered Pipe Thread',(#10796));
#10762=PRODUCT_RELATED_PRODUCT_CATEGORY('Hex Bolt - M6 x 30 mm',
'Hex Bolt - M6 x 30 mm',(#10797));
#10763=PRODUCT_RELATED_PRODUCT_CATEGORY('Valve ball stem and lever',
'Valve ball stem and lever',(#10798));
#10764=PRODUCT_RELATED_PRODUCT_CATEGORY('Ported ball','Ported ball',(#10799));
#10765=PRODUCT_RELATED_PRODUCT_CATEGORY('Stem','Stem',(#10800));
#10766=PRODUCT_RELATED_PRODUCT_CATEGORY('Lever','Lever',(#10801));
#10767=PRODUCT_RELATED_PRODUCT_CATEGORY('Lever keeper','Lever keeper',(#10802));
#10768=PRODUCT_RELATED_PRODUCT_CATEGORY('Bonded grip','Bonded grip',(#10803));
#10769=PRODUCT_RELATED_PRODUCT_CATEGORY('M4x10 Cap Screw',
'M4x10 Cap Screw',(#10804));
#10770=APPLICATION_PROTOCOL_DEFINITION('international standard',
'automotive_design',2009,#10771);
#10771=APPLICATION_CONTEXT(
'Core Data for Automotive Mechanical Design Process');
#10772=PRODUCT_CONTEXT('part definition',#10771,'mechanical');
#10773=PRODUCT('PAT-121','PAT-121',
'PAT-121',(#10772));
#10774=PRODUCT('Bracket pipework and valve body',
'Bracket pipework and valve body','Bracket pipework and valve body',(#10772));
#10775=PRODUCT('Valve port reducer','Valve port reducer',
'Valve port reducer',(#10772));
#10776=PRODUCT('Valve port reducer (1)','Valve port reducer (1)',
'Valve port reducer (1)',(#10772));
#10777=PRODUCT('Wall bracket','Wall bracket','Wall bracket',(#10772));
#10778=PRODUCT('Bulkhead retaining nut','Bulkhead retaining nut',
'Bulkhead retaining nut',(#10772));
#10779=PRODUCT('Hose barb','Hose barb','Hose barb',(#10772));
#10780=PRODUCT('Body inlet half','Body inlet half','Body inlet half',(#10772));
#10781=PRODUCT('Body outlet half','Body outlet half','Body outlet half',
(#10772));
#10782=PRODUCT('Split-body gasket','Split-body gasket',
'Split-body gasket',(#10772));
#10783=PRODUCT('Stem guide','Stem guide','Stem guide',(#10772));
#10784=PRODUCT('Packing ring','Packing ring','Packing ring',(#10772));
#10785=PRODUCT('Packing retainer','Packing retainer','Packing retainer',
(#10772));
#10786=PRODUCT('Lever stop bridge','Lever stop bridge',
'Lever stop bridge',(#10772));
#10787=PRODUCT('Ball seat','Ball seat','Ball seat',(#10772));
#10788=PRODUCT('M5x70 body screw','M5x70 body screw','M5x70 body screw',
(#10772));
#10789=PRODUCT('Flat Washer - M5','Flat Washer - M5','Flat Washer - M5',
(#10772));
#10790=PRODUCT('Hex Nut - M5','Hex Nut - M5','Hex Nut - M5',(#10772));
#10791=PRODUCT('Hex Pipe Nipple - 1-2 Inch Tapered Pipe Thread',
'Hex Pipe Nipple - 1-2 Inch Tapered Pipe Thread',
'Hex Pipe Nipple - 1-2 Inch Tapered Pipe Thread',(#10772));
#10792=PRODUCT('Bridge spacer','Bridge spacer','Bridge spacer',(#10772));
#10793=PRODUCT('Cap Screw - M4x16','Cap Screw - M4x16',
'Cap Screw - M4x16',(#10772));
#10794=PRODUCT('Stop pin','Stop pin','Stop pin',(#10772));
#10795=PRODUCT('Connected quarter-inch elbow',
'Connected quarter-inch elbow','Connected quarter-inch elbow',(#10772));
#10796=PRODUCT('Hex Pipe Nipple - 1-4 Inch Tapered Pipe Thread',
'Hex Pipe Nipple - 1-4 Inch Tapered Pipe Thread',
'Hex Pipe Nipple - 1-4 Inch Tapered Pipe Thread',(#10772));
#10797=PRODUCT('Hex Bolt - M6 x 30 mm','Hex Bolt - M6 x 30 mm',
'Hex Bolt - M6 x 30 mm',(#10772));
#10798=PRODUCT('Valve ball stem and lever','Valve ball stem and lever',
'Valve ball stem and lever',(#10772));
#10799=PRODUCT('Ported ball','Ported ball','Ported ball',(#10772));
#10800=PRODUCT('Stem','Stem','Stem',(#10772));
#10801=PRODUCT('Lever','Lever','Lever',(#10772));
#10802=PRODUCT('Lever keeper','Lever keeper','Lever keeper',(#10772));
#10803=PRODUCT('Bonded grip','Bonded grip','Bonded grip',(#10772));
#10804=PRODUCT('M4x10 Cap Screw','M4x10 Cap Screw','M4x10 Cap Screw',(#10772));
#10805=PRESENTATION_STYLE_ASSIGNMENT((#10811));
#10806=PRESENTATION_STYLE_ASSIGNMENT((#10812));
#10807=PRESENTATION_STYLE_ASSIGNMENT((#10813));
#10808=PRESENTATION_STYLE_ASSIGNMENT((#10814));
#10809=PRESENTATION_STYLE_ASSIGNMENT((#10815));
#10810=PRESENTATION_STYLE_ASSIGNMENT((#10816));
#10811=SURFACE_STYLE_USAGE(.BOTH.,#10817);
#10812=SURFACE_STYLE_USAGE(.BOTH.,#10818);
#10813=SURFACE_STYLE_USAGE(.BOTH.,#10819);
#10814=SURFACE_STYLE_USAGE(.BOTH.,#10820);
#10815=SURFACE_STYLE_USAGE(.BOTH.,#10821);
#10816=SURFACE_STYLE_USAGE(.BOTH.,#10822);
#10817=SURFACE_SIDE_STYLE('',(#10823));
#10818=SURFACE_SIDE_STYLE('',(#10824));
#10819=SURFACE_SIDE_STYLE('',(#10825));
#10820=SURFACE_SIDE_STYLE('',(#10826));
#10821=SURFACE_SIDE_STYLE('',(#10827));
#10822=SURFACE_SIDE_STYLE('',(#10828));
#10823=SURFACE_STYLE_FILL_AREA(#10829);
#10824=SURFACE_STYLE_FILL_AREA(#10830);
#10825=SURFACE_STYLE_FILL_AREA(#10831);
#10826=SURFACE_STYLE_FILL_AREA(#10832);
#10827=SURFACE_STYLE_FILL_AREA(#10833);
#10828=SURFACE_STYLE_FILL_AREA(#10834);
#10829=FILL_AREA_STYLE('Steel - Satin',(#10835));
#10830=FILL_AREA_STYLE('CAD Library Painted - Engineering blue',(#10836));
#10831=FILL_AREA_STYLE('CAD Library Painted - Off white',(#10837));
#10832=FILL_AREA_STYLE('CAD Library Painted - Steel gray',(#10838));
#10833=FILL_AREA_STYLE('CAD Library Painted - Light blue',(#10839));
#10834=FILL_AREA_STYLE('CAD Library Painted - Graphite',(#10840));
#10835=FILL_AREA_STYLE_COLOUR('Steel - Satin',#10841);
#10836=FILL_AREA_STYLE_COLOUR('CAD Library Painted - Engineering blue',
#10842);
#10837=FILL_AREA_STYLE_COLOUR('CAD Library Painted - Off white',#10843);
#10838=FILL_AREA_STYLE_COLOUR('CAD Library Painted - Steel gray',#10844);
#10839=FILL_AREA_STYLE_COLOUR('CAD Library Painted - Light blue',#10845);
#10840=FILL_AREA_STYLE_COLOUR('CAD Library Painted - Graphite',#10846);
#10841=COLOUR_RGB('Steel - Satin',0.627450980392157,0.627450980392157,0.627450980392157);
#10842=COLOUR_RGB('CAD Library Painted - Engineering blue',0.12156862745098,
0.356862745098039,0.6);
#10843=COLOUR_RGB('CAD Library Painted - Off white',0.909803921568627,0.901960784313726,
0.858823529411765);
#10844=COLOUR_RGB('CAD Library Painted - Steel gray',0.592156862745098,
0.631372549019608,0.67843137254902);
#10845=COLOUR_RGB('CAD Library Painted - Light blue',0.286274509803922,
0.552941176470588,0.780392156862745);
#10846=COLOUR_RGB('CAD Library Painted - Graphite',0.0980392156862745,0.109803921568627,
0.125490196078431);
#10847=COLOUR_RGB('Dark Blue',0.08,0.2,0.34);
#10848=FILL_AREA_STYLE_COLOUR('',#10847);
#10849=FILL_AREA_STYLE('',(#10848));
#10850=SURFACE_STYLE_FILL_AREA(#10849);
#10851=SURFACE_SIDE_STYLE('',(#10850));
#10852=SURFACE_STYLE_USAGE(.BOTH.,#10851);
#10853=PRESENTATION_STYLE_ASSIGNMENT((#10852));
#10854=COLOUR_RGB('Light Blue',0.38,0.62,0.78);
#10855=FILL_AREA_STYLE_COLOUR('',#10854);
#10856=FILL_AREA_STYLE('',(#10855));
#10857=SURFACE_STYLE_FILL_AREA(#10856);
#10858=SURFACE_SIDE_STYLE('',(#10857));
#10859=SURFACE_STYLE_USAGE(.BOTH.,#10858);
#10860=PRESENTATION_STYLE_ASSIGNMENT((#10859));
#10861=COLOUR_RGB('Sky Blue',0.24,0.69,0.87);
#10862=FILL_AREA_STYLE_COLOUR('',#10861);
#10863=FILL_AREA_STYLE('',(#10862));
#10864=SURFACE_STYLE_FILL_AREA(#10863);
#10865=SURFACE_SIDE_STYLE('',(#10864));
#10866=SURFACE_STYLE_USAGE(.BOTH.,#10865);
#10867=PRESENTATION_STYLE_ASSIGNMENT((#10866));
#10868=COLOUR_RGB('Grey',0.48,0.52,0.57);
#10869=FILL_AREA_STYLE_COLOUR('',#10868);
#10870=FILL_AREA_STYLE('',(#10869));
#10871=SURFACE_STYLE_FILL_AREA(#10870);
#10872=SURFACE_SIDE_STYLE('',(#10871));
#10873=SURFACE_STYLE_USAGE(.BOTH.,#10872);
#10874=PRESENTATION_STYLE_ASSIGNMENT((#10873));
#10875=COLOUR_RGB('Black',0.12,0.14,0.17);
#10876=FILL_AREA_STYLE_COLOUR('',#10875);
#10877=FILL_AREA_STYLE('',(#10876));
#10878=SURFACE_STYLE_FILL_AREA(#10877);
#10879=SURFACE_SIDE_STYLE('',(#10878));
#10880=SURFACE_STYLE_USAGE(.BOTH.,#10879);
#10881=PRESENTATION_STYLE_ASSIGNMENT((#10880));
#10882=COLOUR_RGB('Off White',0.89,0.88,0.83);
#10883=FILL_AREA_STYLE_COLOUR('',#10882);
#10884=FILL_AREA_STYLE('',(#10883));
#10885=SURFACE_STYLE_FILL_AREA(#10884);
#10886=SURFACE_SIDE_STYLE('',(#10885));
#10887=SURFACE_STYLE_USAGE(.BOTH.,#10886);
#10888=PRESENTATION_STYLE_ASSIGNMENT((#10887));
ENDSEC;
END-ISO-10303-21;
